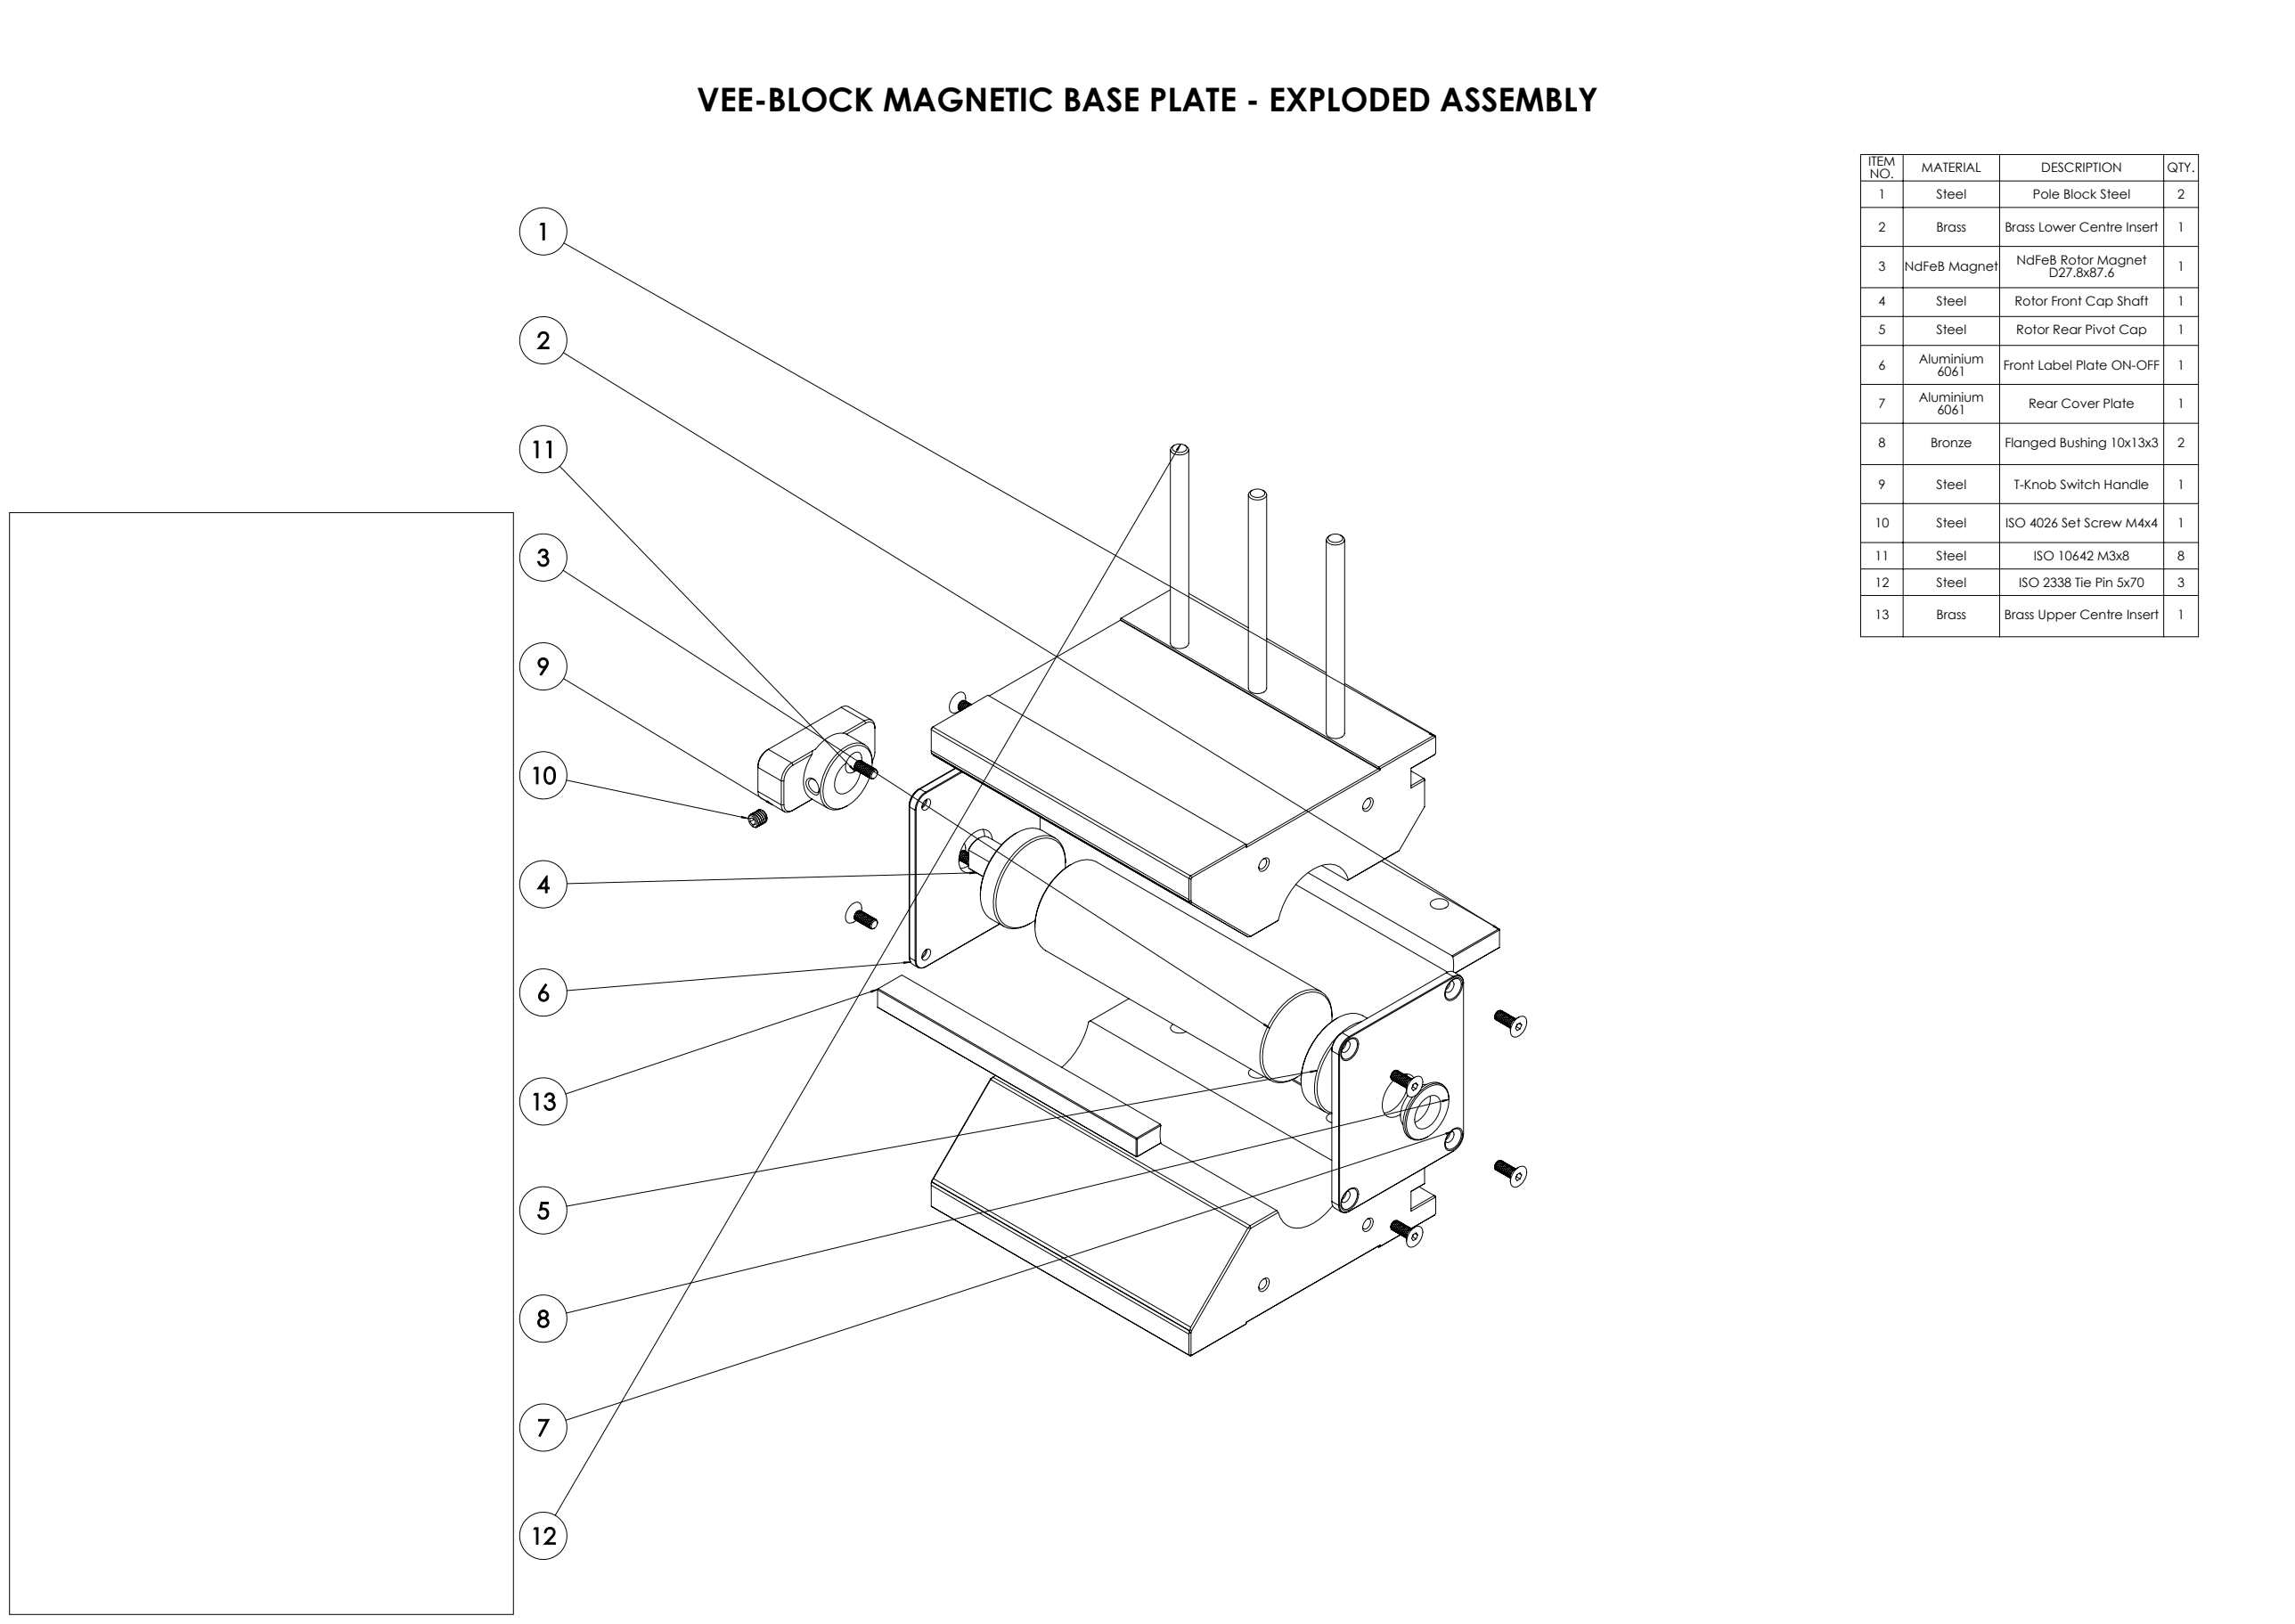
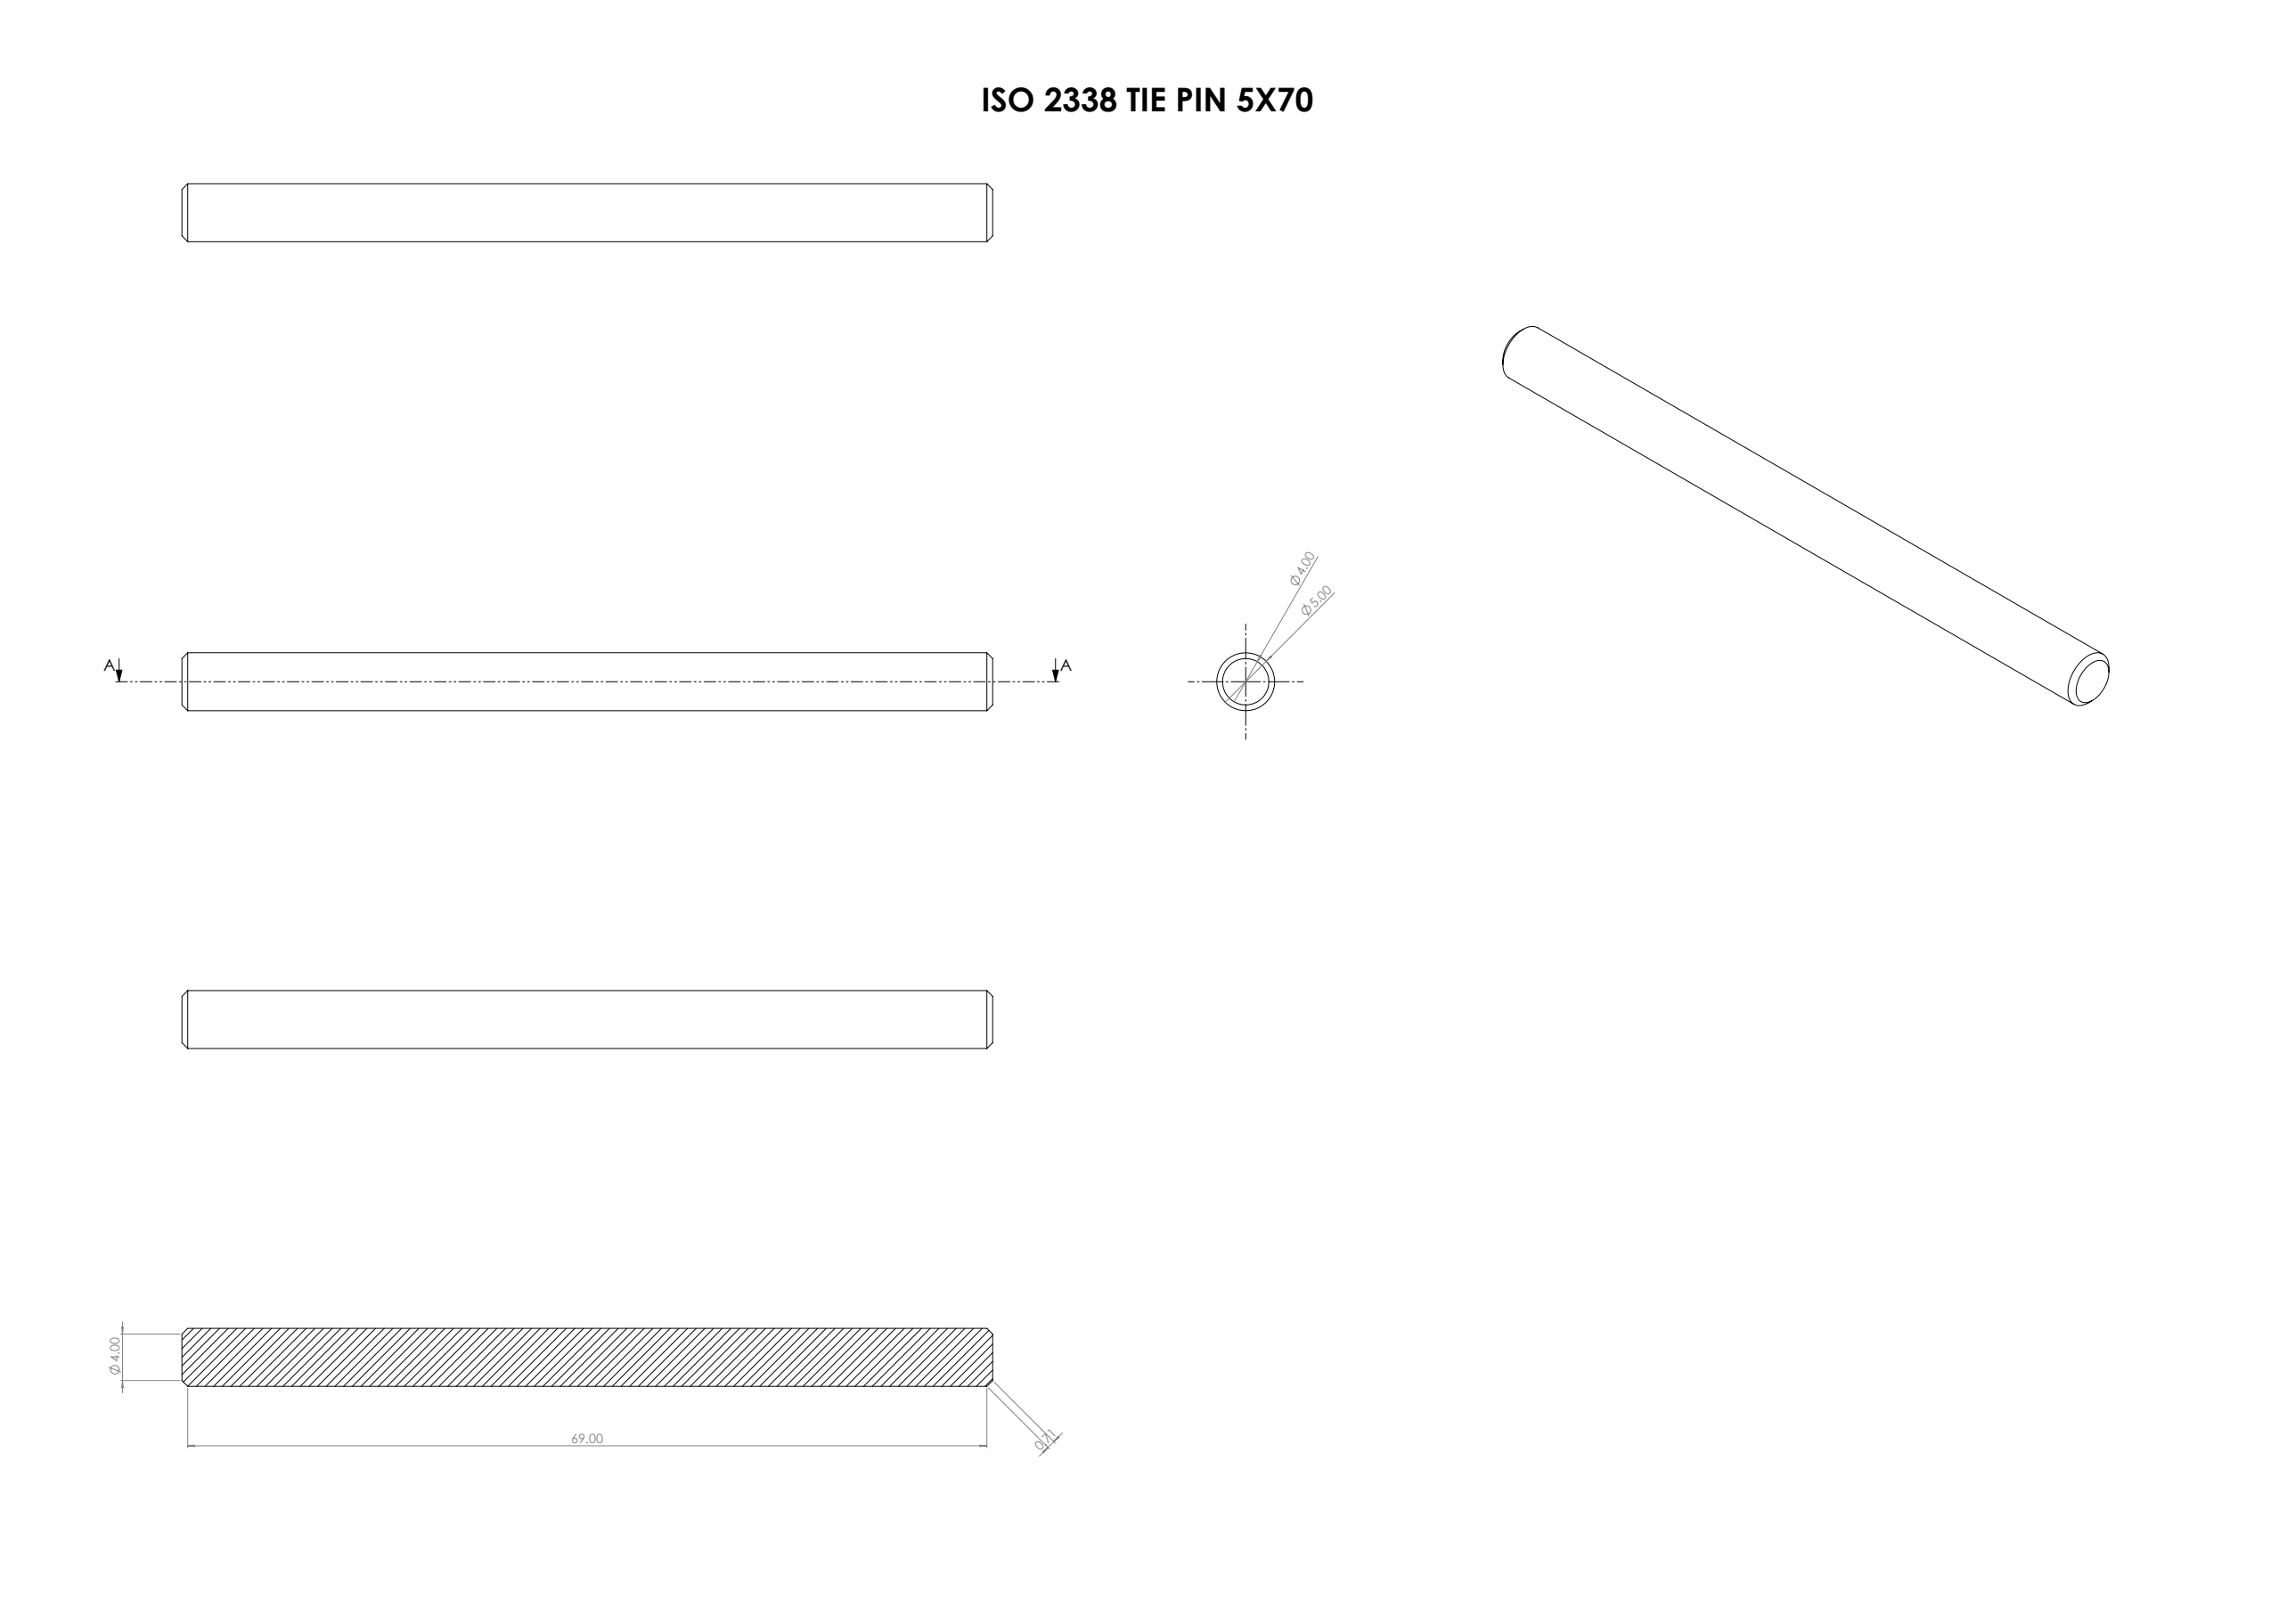
ISO-10303-21;
HEADER;
/* Generated by software containing ST-Developer
 * from STEP Tools, Inc. (www.steptools.com) 
 */

FILE_DESCRIPTION(
/* description */ (''),
/* implementation_level */ '2;1');

FILE_NAME(
/* name */ 'MAS-286',
/* time_stamp */ '2026-10-21T01:59:45-07:00',
/* author */ (''),
/* organization */ (''),
/* preprocessor_version */ 'ST-DEVELOPER v20.2',
/* originating_system */ 'Autodesk Translation Framework v15.15.0.0',
/* authorisation */ '');

FILE_SCHEMA (('AUTOMOTIVE_DESIGN { 1 0 10303 214 3 1 1 }'));
ENDSEC;

DATA;
#10=MECHANICAL_DESIGN_GEOMETRIC_PRESENTATION_REPRESENTATION('',(#463,#464,
#465,#466,#467,#468,#469,#470,#471,#472,#473,#474,#475,#476,#477,#478,#479,
#480),#18281);
#11=ITEM_DEFINED_TRANSFORMATION($,$,#9544,#9946);
#12=ITEM_DEFINED_TRANSFORMATION($,$,#9243,#9947);
#13=ITEM_DEFINED_TRANSFORMATION($,$,#9277,#9948);
#14=ITEM_DEFINED_TRANSFORMATION($,$,#9302,#9949);
#15=ITEM_DEFINED_TRANSFORMATION($,$,#9470,#9950);
#16=ITEM_DEFINED_TRANSFORMATION($,$,#9544,#9951);
#17=ITEM_DEFINED_TRANSFORMATION($,$,#9664,#9952);
#18=ITEM_DEFINED_TRANSFORMATION($,$,#9674,#9953);
#19=ITEM_DEFINED_TRANSFORMATION($,$,#9696,#9954);
#20=ITEM_DEFINED_TRANSFORMATION($,$,#9713,#9955);
#21=ITEM_DEFINED_TRANSFORMATION($,$,#9713,#9956);
#22=ITEM_DEFINED_TRANSFORMATION($,$,#9729,#9957);
#23=ITEM_DEFINED_TRANSFORMATION($,$,#9847,#9958);
#24=ITEM_DEFINED_TRANSFORMATION($,$,#9884,#9959);
#25=ITEM_DEFINED_TRANSFORMATION($,$,#9884,#9960);
#26=ITEM_DEFINED_TRANSFORMATION($,$,#9884,#9961);
#27=ITEM_DEFINED_TRANSFORMATION($,$,#9884,#9962);
#28=ITEM_DEFINED_TRANSFORMATION($,$,#9884,#9963);
#29=ITEM_DEFINED_TRANSFORMATION($,$,#9884,#9964);
#30=ITEM_DEFINED_TRANSFORMATION($,$,#9884,#9965);
#31=ITEM_DEFINED_TRANSFORMATION($,$,#9884,#9966);
#32=ITEM_DEFINED_TRANSFORMATION($,$,#9936,#9967);
#33=ITEM_DEFINED_TRANSFORMATION($,$,#9936,#9968);
#34=ITEM_DEFINED_TRANSFORMATION($,$,#9936,#9969);
#35=(
REPRESENTATION_RELATIONSHIP($,$,#18343,#18338)
REPRESENTATION_RELATIONSHIP_WITH_TRANSFORMATION(#11)
SHAPE_REPRESENTATION_RELATIONSHIP()
);
#36=(
REPRESENTATION_RELATIONSHIP($,$,#18339,#18338)
REPRESENTATION_RELATIONSHIP_WITH_TRANSFORMATION(#12)
SHAPE_REPRESENTATION_RELATIONSHIP()
);
#37=(
REPRESENTATION_RELATIONSHIP($,$,#18340,#18338)
REPRESENTATION_RELATIONSHIP_WITH_TRANSFORMATION(#13)
SHAPE_REPRESENTATION_RELATIONSHIP()
);
#38=(
REPRESENTATION_RELATIONSHIP($,$,#18341,#18338)
REPRESENTATION_RELATIONSHIP_WITH_TRANSFORMATION(#14)
SHAPE_REPRESENTATION_RELATIONSHIP()
);
#39=(
REPRESENTATION_RELATIONSHIP($,$,#18342,#18338)
REPRESENTATION_RELATIONSHIP_WITH_TRANSFORMATION(#15)
SHAPE_REPRESENTATION_RELATIONSHIP()
);
#40=(
REPRESENTATION_RELATIONSHIP($,$,#18343,#18338)
REPRESENTATION_RELATIONSHIP_WITH_TRANSFORMATION(#16)
SHAPE_REPRESENTATION_RELATIONSHIP()
);
#41=(
REPRESENTATION_RELATIONSHIP($,$,#18344,#18338)
REPRESENTATION_RELATIONSHIP_WITH_TRANSFORMATION(#17)
SHAPE_REPRESENTATION_RELATIONSHIP()
);
#42=(
REPRESENTATION_RELATIONSHIP($,$,#18345,#18338)
REPRESENTATION_RELATIONSHIP_WITH_TRANSFORMATION(#18)
SHAPE_REPRESENTATION_RELATIONSHIP()
);
#43=(
REPRESENTATION_RELATIONSHIP($,$,#18346,#18338)
REPRESENTATION_RELATIONSHIP_WITH_TRANSFORMATION(#19)
SHAPE_REPRESENTATION_RELATIONSHIP()
);
#44=(
REPRESENTATION_RELATIONSHIP($,$,#18347,#18338)
REPRESENTATION_RELATIONSHIP_WITH_TRANSFORMATION(#20)
SHAPE_REPRESENTATION_RELATIONSHIP()
);
#45=(
REPRESENTATION_RELATIONSHIP($,$,#18347,#18338)
REPRESENTATION_RELATIONSHIP_WITH_TRANSFORMATION(#21)
SHAPE_REPRESENTATION_RELATIONSHIP()
);
#46=(
REPRESENTATION_RELATIONSHIP($,$,#18348,#18338)
REPRESENTATION_RELATIONSHIP_WITH_TRANSFORMATION(#22)
SHAPE_REPRESENTATION_RELATIONSHIP()
);
#47=(
REPRESENTATION_RELATIONSHIP($,$,#18349,#18338)
REPRESENTATION_RELATIONSHIP_WITH_TRANSFORMATION(#23)
SHAPE_REPRESENTATION_RELATIONSHIP()
);
#48=(
REPRESENTATION_RELATIONSHIP($,$,#18350,#18338)
REPRESENTATION_RELATIONSHIP_WITH_TRANSFORMATION(#24)
SHAPE_REPRESENTATION_RELATIONSHIP()
);
#49=(
REPRESENTATION_RELATIONSHIP($,$,#18350,#18338)
REPRESENTATION_RELATIONSHIP_WITH_TRANSFORMATION(#25)
SHAPE_REPRESENTATION_RELATIONSHIP()
);
#50=(
REPRESENTATION_RELATIONSHIP($,$,#18350,#18338)
REPRESENTATION_RELATIONSHIP_WITH_TRANSFORMATION(#26)
SHAPE_REPRESENTATION_RELATIONSHIP()
);
#51=(
REPRESENTATION_RELATIONSHIP($,$,#18350,#18338)
REPRESENTATION_RELATIONSHIP_WITH_TRANSFORMATION(#27)
SHAPE_REPRESENTATION_RELATIONSHIP()
);
#52=(
REPRESENTATION_RELATIONSHIP($,$,#18350,#18338)
REPRESENTATION_RELATIONSHIP_WITH_TRANSFORMATION(#28)
SHAPE_REPRESENTATION_RELATIONSHIP()
);
#53=(
REPRESENTATION_RELATIONSHIP($,$,#18350,#18338)
REPRESENTATION_RELATIONSHIP_WITH_TRANSFORMATION(#29)
SHAPE_REPRESENTATION_RELATIONSHIP()
);
#54=(
REPRESENTATION_RELATIONSHIP($,$,#18350,#18338)
REPRESENTATION_RELATIONSHIP_WITH_TRANSFORMATION(#30)
SHAPE_REPRESENTATION_RELATIONSHIP()
);
#55=(
REPRESENTATION_RELATIONSHIP($,$,#18350,#18338)
REPRESENTATION_RELATIONSHIP_WITH_TRANSFORMATION(#31)
SHAPE_REPRESENTATION_RELATIONSHIP()
);
#56=(
REPRESENTATION_RELATIONSHIP($,$,#18351,#18338)
REPRESENTATION_RELATIONSHIP_WITH_TRANSFORMATION(#32)
SHAPE_REPRESENTATION_RELATIONSHIP()
);
#57=(
REPRESENTATION_RELATIONSHIP($,$,#18351,#18338)
REPRESENTATION_RELATIONSHIP_WITH_TRANSFORMATION(#33)
SHAPE_REPRESENTATION_RELATIONSHIP()
);
#58=(
REPRESENTATION_RELATIONSHIP($,$,#18351,#18338)
REPRESENTATION_RELATIONSHIP_WITH_TRANSFORMATION(#34)
SHAPE_REPRESENTATION_RELATIONSHIP()
);
#59=CONTEXT_DEPENDENT_SHAPE_REPRESENTATION(#35,#18314);
#60=CONTEXT_DEPENDENT_SHAPE_REPRESENTATION(#36,#18315);
#61=CONTEXT_DEPENDENT_SHAPE_REPRESENTATION(#37,#18316);
#62=CONTEXT_DEPENDENT_SHAPE_REPRESENTATION(#38,#18317);
#63=CONTEXT_DEPENDENT_SHAPE_REPRESENTATION(#39,#18318);
#64=CONTEXT_DEPENDENT_SHAPE_REPRESENTATION(#40,#18319);
#65=CONTEXT_DEPENDENT_SHAPE_REPRESENTATION(#41,#18320);
#66=CONTEXT_DEPENDENT_SHAPE_REPRESENTATION(#42,#18321);
#67=CONTEXT_DEPENDENT_SHAPE_REPRESENTATION(#43,#18322);
#68=CONTEXT_DEPENDENT_SHAPE_REPRESENTATION(#44,#18323);
#69=CONTEXT_DEPENDENT_SHAPE_REPRESENTATION(#45,#18324);
#70=CONTEXT_DEPENDENT_SHAPE_REPRESENTATION(#46,#18325);
#71=CONTEXT_DEPENDENT_SHAPE_REPRESENTATION(#47,#18326);
#72=CONTEXT_DEPENDENT_SHAPE_REPRESENTATION(#48,#18327);
#73=CONTEXT_DEPENDENT_SHAPE_REPRESENTATION(#49,#18328);
#74=CONTEXT_DEPENDENT_SHAPE_REPRESENTATION(#50,#18329);
#75=CONTEXT_DEPENDENT_SHAPE_REPRESENTATION(#51,#18330);
#76=CONTEXT_DEPENDENT_SHAPE_REPRESENTATION(#52,#18331);
#77=CONTEXT_DEPENDENT_SHAPE_REPRESENTATION(#53,#18332);
#78=CONTEXT_DEPENDENT_SHAPE_REPRESENTATION(#54,#18333);
#79=CONTEXT_DEPENDENT_SHAPE_REPRESENTATION(#55,#18334);
#80=CONTEXT_DEPENDENT_SHAPE_REPRESENTATION(#56,#18335);
#81=CONTEXT_DEPENDENT_SHAPE_REPRESENTATION(#57,#18336);
#82=CONTEXT_DEPENDENT_SHAPE_REPRESENTATION(#58,#18337);
#83=NEXT_ASSEMBLY_USAGE_OCCURRENCE('01_Pole_Block_Steel:1',
'01_Pole_Block_Steel:1','01_Pole_Block_Steel:1',#18353,#18358,
'01_Pole_Block_Steel:1');
#84=NEXT_ASSEMBLY_USAGE_OCCURRENCE('02_Brass_Lower_Centre_Insert:1',
'02_Brass_Lower_Centre_Insert:1','02_Brass_Lower_Centre_Insert:1',#18353,
#18354,'02_Brass_Lower_Centre_Insert:1');
#85=NEXT_ASSEMBLY_USAGE_OCCURRENCE('13_Brass_Upper_Centre_Insert:1',
'13_Brass_Upper_Centre_Insert:1','13_Brass_Upper_Centre_Insert:1',#18353,
#18355,'13_Brass_Upper_Centre_Insert:1');
#86=NEXT_ASSEMBLY_USAGE_OCCURRENCE('06_Front_Label_Plate_ON-OFF:1',
'06_Front_Label_Plate_ON-OFF:1','06_Front_Label_Plate_ON-OFF:1',#18353,
#18356,'06_Front_Label_Plate_ON-OFF:1');
#87=NEXT_ASSEMBLY_USAGE_OCCURRENCE('07_Rear_Cover_Plate:1',
'07_Rear_Cover_Plate:1','07_Rear_Cover_Plate:1',#18353,#18357,
'07_Rear_Cover_Plate:1');
#88=NEXT_ASSEMBLY_USAGE_OCCURRENCE('01_Pole_Block_Steel:2',
'01_Pole_Block_Steel:2','01_Pole_Block_Steel:2',#18353,#18358,
'01_Pole_Block_Steel:2');
#89=NEXT_ASSEMBLY_USAGE_OCCURRENCE('03_NdFeB_Rotor_Magnet_D27.8x87.6:2',
'03_NdFeB_Rotor_Magnet_D27.8x87.6:2',
'03_NdFeB_Rotor_Magnet_D27.8x87.6:2',#18353,#18359,
'03_NdFeB_Rotor_Magnet_D27.8x87.6:2');
#90=NEXT_ASSEMBLY_USAGE_OCCURRENCE('04_Rotor_Front_Cap_Shaft:2',
'04_Rotor_Front_Cap_Shaft:2','04_Rotor_Front_Cap_Shaft:2',#18353,#18360,
'04_Rotor_Front_Cap_Shaft:2');
#91=NEXT_ASSEMBLY_USAGE_OCCURRENCE('05_Rotor_Rear_Pivot_Cap:2',
'05_Rotor_Rear_Pivot_Cap:2','05_Rotor_Rear_Pivot_Cap:2',#18353,#18361,
'05_Rotor_Rear_Pivot_Cap:2');
#92=NEXT_ASSEMBLY_USAGE_OCCURRENCE('08_Flanged_Bushing_10x13x3:2',
'08_Flanged_Bushing_10x13x3:2','08_Flanged_Bushing_10x13x3:2',#18353,#18362,
'08_Flanged_Bushing_10x13x3:2');
#93=NEXT_ASSEMBLY_USAGE_OCCURRENCE('08_Flanged_Bushing_10x13x3:3',
'08_Flanged_Bushing_10x13x3:3','08_Flanged_Bushing_10x13x3:3',#18353,#18362,
'08_Flanged_Bushing_10x13x3:3');
#94=NEXT_ASSEMBLY_USAGE_OCCURRENCE('09_T-Knob_Switch_Handle:2',
'09_T-Knob_Switch_Handle:2','09_T-Knob_Switch_Handle:2',#18353,#18363,
'09_T-Knob_Switch_Handle:2');
#95=NEXT_ASSEMBLY_USAGE_OCCURRENCE('10_ISO_4026_Set_Screw_M4x4:2',
'10_ISO_4026_Set_Screw_M4x4:2','10_ISO_4026_Set_Screw_M4x4:2',#18353,#18364,
'10_ISO_4026_Set_Screw_M4x4:2');
#96=NEXT_ASSEMBLY_USAGE_OCCURRENCE('11_ISO_10642_M3x8:2',
'11_ISO_10642_M3x8:2','11_ISO_10642_M3x8:2',#18353,#18365,
'11_ISO_10642_M3x8:2');
#97=NEXT_ASSEMBLY_USAGE_OCCURRENCE('11_ISO_10642_M3x8:3',
'11_ISO_10642_M3x8:3','11_ISO_10642_M3x8:3',#18353,#18365,
'11_ISO_10642_M3x8:3');
#98=NEXT_ASSEMBLY_USAGE_OCCURRENCE('11_ISO_10642_M3x8:4',
'11_ISO_10642_M3x8:4','11_ISO_10642_M3x8:4',#18353,#18365,
'11_ISO_10642_M3x8:4');
#99=NEXT_ASSEMBLY_USAGE_OCCURRENCE('11_ISO_10642_M3x8:5',
'11_ISO_10642_M3x8:5','11_ISO_10642_M3x8:5',#18353,#18365,
'11_ISO_10642_M3x8:5');
#100=NEXT_ASSEMBLY_USAGE_OCCURRENCE('11_ISO_10642_M3x8:6',
'11_ISO_10642_M3x8:6','11_ISO_10642_M3x8:6',#18353,#18365,
'11_ISO_10642_M3x8:6');
#101=NEXT_ASSEMBLY_USAGE_OCCURRENCE('11_ISO_10642_M3x8:7',
'11_ISO_10642_M3x8:7','11_ISO_10642_M3x8:7',#18353,#18365,
'11_ISO_10642_M3x8:7');
#102=NEXT_ASSEMBLY_USAGE_OCCURRENCE('11_ISO_10642_M3x8:8',
'11_ISO_10642_M3x8:8','11_ISO_10642_M3x8:8',#18353,#18365,
'11_ISO_10642_M3x8:8');
#103=NEXT_ASSEMBLY_USAGE_OCCURRENCE('11_ISO_10642_M3x8:9',
'11_ISO_10642_M3x8:9','11_ISO_10642_M3x8:9',#18353,#18365,
'11_ISO_10642_M3x8:9');
#104=NEXT_ASSEMBLY_USAGE_OCCURRENCE('12_ISO_2338_Tie_Pin_5x70:2',
'12_ISO_2338_Tie_Pin_5x70:2','12_ISO_2338_Tie_Pin_5x70:2',#18353,#18366,
'12_ISO_2338_Tie_Pin_5x70:2');
#105=NEXT_ASSEMBLY_USAGE_OCCURRENCE('12_ISO_2338_Tie_Pin_5x70:3',
'12_ISO_2338_Tie_Pin_5x70:3','12_ISO_2338_Tie_Pin_5x70:3',#18353,#18366,
'12_ISO_2338_Tie_Pin_5x70:3');
#106=NEXT_ASSEMBLY_USAGE_OCCURRENCE('12_ISO_2338_Tie_Pin_5x70:4',
'12_ISO_2338_Tie_Pin_5x70:4','12_ISO_2338_Tie_Pin_5x70:4',#18353,#18366,
'12_ISO_2338_Tie_Pin_5x70:4');
#107=(
BOUNDED_CURVE()
B_SPLINE_CURVE(2,(#12695,#12696,#12697),.UNSPECIFIED.,.F.,.F.)
B_SPLINE_CURVE_WITH_KNOTS((3,3),(0.,0.110982483350979),.UNSPECIFIED.)
CURVE()
GEOMETRIC_REPRESENTATION_ITEM()
RATIONAL_B_SPLINE_CURVE((1.,1.,1.))
REPRESENTATION_ITEM('')
);
#108=(
BOUNDED_CURVE()
B_SPLINE_CURVE(2,(#12710,#12711,#12712),.UNSPECIFIED.,.F.,.F.)
B_SPLINE_CURVE_WITH_KNOTS((3,3),(0.058586025044114,0.117172050088227),
 .UNSPECIFIED.)
CURVE()
GEOMETRIC_REPRESENTATION_ITEM()
RATIONAL_B_SPLINE_CURVE((1.,1.,1.))
REPRESENTATION_ITEM('')
);
#109=(
BOUNDED_CURVE()
B_SPLINE_CURVE(2,(#12739,#12740,#12741),.UNSPECIFIED.,.F.,.F.)
B_SPLINE_CURVE_WITH_KNOTS((3,3),(0.,0.0585860250441136),.UNSPECIFIED.)
CURVE()
GEOMETRIC_REPRESENTATION_ITEM()
RATIONAL_B_SPLINE_CURVE((1.,1.,1.))
REPRESENTATION_ITEM('')
);
#110=(
BOUNDED_CURVE()
B_SPLINE_CURVE(2,(#12754,#12755,#12756),.UNSPECIFIED.,.F.,.F.)
B_SPLINE_CURVE_WITH_KNOTS((3,3),(0.0909175021833372,0.201899986183551),
 .UNSPECIFIED.)
CURVE()
GEOMETRIC_REPRESENTATION_ITEM()
RATIONAL_B_SPLINE_CURVE((1.,1.,1.))
REPRESENTATION_ITEM('')
);
#111=(
BOUNDED_CURVE()
B_SPLINE_CURVE(2,(#12765,#12766,#12767),.UNSPECIFIED.,.F.,.F.)
B_SPLINE_CURVE_WITH_KNOTS((3,3),(0.0485753412182672,0.117172050088219),
 .UNSPECIFIED.)
CURVE()
GEOMETRIC_REPRESENTATION_ITEM()
RATIONAL_B_SPLINE_CURVE((1.,1.,1.))
REPRESENTATION_ITEM('')
);
#112=(
BOUNDED_CURVE()
B_SPLINE_CURVE(2,(#12779,#12780,#12781),.UNSPECIFIED.,.F.,.F.)
B_SPLINE_CURVE_WITH_KNOTS((3,3),(0.0585860250445827,0.117172050088221),
 .UNSPECIFIED.)
CURVE()
GEOMETRIC_REPRESENTATION_ITEM()
RATIONAL_B_SPLINE_CURVE((1.,1.,1.))
REPRESENTATION_ITEM('')
);
#113=(
BOUNDED_CURVE()
B_SPLINE_CURVE(2,(#12785,#12786,#12787),.UNSPECIFIED.,.F.,.F.)
B_SPLINE_CURVE_WITH_KNOTS((3,3),(0.,0.068596708869952),.UNSPECIFIED.)
CURVE()
GEOMETRIC_REPRESENTATION_ITEM()
RATIONAL_B_SPLINE_CURVE((1.,1.,1.))
REPRESENTATION_ITEM('')
);
#114=(
BOUNDED_CURVE()
B_SPLINE_CURVE(2,(#12799,#12800,#12801),.UNSPECIFIED.,.F.,.F.)
B_SPLINE_CURVE_WITH_KNOTS((3,3),(0.0485753412182676,0.0585860250445827),
 .UNSPECIFIED.)
CURVE()
GEOMETRIC_REPRESENTATION_ITEM()
RATIONAL_B_SPLINE_CURVE((1.,1.,1.))
REPRESENTATION_ITEM('')
);
#115=(
BOUNDED_CURVE()
B_SPLINE_CURVE(2,(#13088,#13089,#13090),.UNSPECIFIED.,.F.,.F.)
B_SPLINE_CURVE_WITH_KNOTS((3,3),(0.058586025043638,0.0685967088699541),
 .UNSPECIFIED.)
CURVE()
GEOMETRIC_REPRESENTATION_ITEM()
RATIONAL_B_SPLINE_CURVE((1.,1.,1.))
REPRESENTATION_ITEM('')
);
#116=(
BOUNDED_CURVE()
B_SPLINE_CURVE(2,(#13101,#13102,#13103),.UNSPECIFIED.,.F.,.F.)
B_SPLINE_CURVE_WITH_KNOTS((3,3),(0.,0.058586025043638),.UNSPECIFIED.)
CURVE()
GEOMETRIC_REPRESENTATION_ITEM()
RATIONAL_B_SPLINE_CURVE((1.,1.,1.))
REPRESENTATION_ITEM('')
);
#117=(
BOUNDED_CURVE()
B_SPLINE_CURVE(2,(#14471,#14472,#14473),.UNSPECIFIED.,.F.,.F.)
B_SPLINE_CURVE_WITH_KNOTS((3,3),(0.,0.0727628528393549),.UNSPECIFIED.)
CURVE()
GEOMETRIC_REPRESENTATION_ITEM()
RATIONAL_B_SPLINE_CURVE((1.,1.,1.))
REPRESENTATION_ITEM('')
);
#118=(
BOUNDED_CURVE()
B_SPLINE_CURVE(2,(#14477,#14478,#14479),.UNSPECIFIED.,.F.,.F.)
B_SPLINE_CURVE_WITH_KNOTS((3,3),(0.,0.0727628528393549),.UNSPECIFIED.)
CURVE()
GEOMETRIC_REPRESENTATION_ITEM()
RATIONAL_B_SPLINE_CURVE((1.,1.,1.))
REPRESENTATION_ITEM('')
);
#119=(
BOUNDED_CURVE()
B_SPLINE_CURVE(2,(#14814,#14815,#14816),.UNSPECIFIED.,.F.,.F.)
B_SPLINE_CURVE_WITH_KNOTS((3,3),(0.,0.0729284032695322),.UNSPECIFIED.)
CURVE()
GEOMETRIC_REPRESENTATION_ITEM()
RATIONAL_B_SPLINE_CURVE((1.,1.,1.))
REPRESENTATION_ITEM('')
);
#120=(
BOUNDED_CURVE()
B_SPLINE_CURVE(2,(#14820,#14821,#14822),.UNSPECIFIED.,.F.,.F.)
B_SPLINE_CURVE_WITH_KNOTS((3,3),(0.,0.072928403269532),.UNSPECIFIED.)
CURVE()
GEOMETRIC_REPRESENTATION_ITEM()
RATIONAL_B_SPLINE_CURVE((1.,1.,1.))
REPRESENTATION_ITEM('')
);
#121=(
BOUNDED_CURVE()
B_SPLINE_CURVE(2,(#14826,#14827,#14828),.UNSPECIFIED.,.F.,.F.)
B_SPLINE_CURVE_WITH_KNOTS((3,3),(0.,0.0457691166614135),.UNSPECIFIED.)
CURVE()
GEOMETRIC_REPRESENTATION_ITEM()
RATIONAL_B_SPLINE_CURVE((1.,1.,1.))
REPRESENTATION_ITEM('')
);
#122=(
BOUNDED_CURVE()
B_SPLINE_CURVE(2,(#14831,#14832,#14833),.UNSPECIFIED.,.F.,.F.)
B_SPLINE_CURVE_WITH_KNOTS((3,3),(0.,0.0457691166614134),.UNSPECIFIED.)
CURVE()
GEOMETRIC_REPRESENTATION_ITEM()
RATIONAL_B_SPLINE_CURVE((1.,1.,1.))
REPRESENTATION_ITEM('')
);
#123=(
BOUNDED_CURVE()
B_SPLINE_CURVE(2,(#14897,#14898,#14899),.UNSPECIFIED.,.F.,.F.)
B_SPLINE_CURVE_WITH_KNOTS((3,3),(0.,0.0577818255968905),.UNSPECIFIED.)
CURVE()
GEOMETRIC_REPRESENTATION_ITEM()
RATIONAL_B_SPLINE_CURVE((1.,1.,1.))
REPRESENTATION_ITEM('')
);
#124=(
BOUNDED_CURVE()
B_SPLINE_CURVE(2,(#14903,#14904,#14905),.UNSPECIFIED.,.F.,.F.)
B_SPLINE_CURVE_WITH_KNOTS((3,3),(0.,0.0577818255968905),.UNSPECIFIED.)
CURVE()
GEOMETRIC_REPRESENTATION_ITEM()
RATIONAL_B_SPLINE_CURVE((1.,1.,1.))
REPRESENTATION_ITEM('')
);
#125=(
BOUNDED_CURVE()
B_SPLINE_CURVE(2,(#14909,#14910,#14911),.UNSPECIFIED.,.F.,.F.)
B_SPLINE_CURVE_WITH_KNOTS((3,3),(0.,0.0492830096737056),.UNSPECIFIED.)
CURVE()
GEOMETRIC_REPRESENTATION_ITEM()
RATIONAL_B_SPLINE_CURVE((1.,1.,1.))
REPRESENTATION_ITEM('')
);
#126=(
BOUNDED_CURVE()
B_SPLINE_CURVE(2,(#14914,#14915,#14916),.UNSPECIFIED.,.F.,.F.)
B_SPLINE_CURVE_WITH_KNOTS((3,3),(0.,0.0492830096737056),.UNSPECIFIED.)
CURVE()
GEOMETRIC_REPRESENTATION_ITEM()
RATIONAL_B_SPLINE_CURVE((1.,1.,1.))
REPRESENTATION_ITEM('')
);
#127=(
BOUNDED_CURVE()
B_SPLINE_CURVE(2,(#14920,#14921,#14922),.UNSPECIFIED.,.F.,.F.)
B_SPLINE_CURVE_WITH_KNOTS((3,3),(0.,0.072928403269532),.UNSPECIFIED.)
CURVE()
GEOMETRIC_REPRESENTATION_ITEM()
RATIONAL_B_SPLINE_CURVE((1.,1.,1.))
REPRESENTATION_ITEM('')
);
#128=(
BOUNDED_CURVE()
B_SPLINE_CURVE(2,(#14926,#14927,#14928),.UNSPECIFIED.,.F.,.F.)
B_SPLINE_CURVE_WITH_KNOTS((3,3),(0.,0.0729284032695322),.UNSPECIFIED.)
CURVE()
GEOMETRIC_REPRESENTATION_ITEM()
RATIONAL_B_SPLINE_CURVE((1.,1.,1.))
REPRESENTATION_ITEM('')
);
#129=(
BOUNDED_CURVE()
B_SPLINE_CURVE(2,(#14932,#14933,#14934),.UNSPECIFIED.,.F.,.F.)
B_SPLINE_CURVE_WITH_KNOTS((3,3),(0.,0.0457691166614135),.UNSPECIFIED.)
CURVE()
GEOMETRIC_REPRESENTATION_ITEM()
RATIONAL_B_SPLINE_CURVE((1.,1.,1.))
REPRESENTATION_ITEM('')
);
#130=(
BOUNDED_CURVE()
B_SPLINE_CURVE(2,(#14937,#14938,#14939),.UNSPECIFIED.,.F.,.F.)
B_SPLINE_CURVE_WITH_KNOTS((3,3),(0.,0.0457691166614134),.UNSPECIFIED.)
CURVE()
GEOMETRIC_REPRESENTATION_ITEM()
RATIONAL_B_SPLINE_CURVE((1.,1.,1.))
REPRESENTATION_ITEM('')
);
#131=(
BOUNDED_CURVE()
B_SPLINE_CURVE(2,(#14973,#14974,#14975),.UNSPECIFIED.,.F.,.F.)
B_SPLINE_CURVE_WITH_KNOTS((3,3),(0.,0.210313307559557),.UNSPECIFIED.)
CURVE()
GEOMETRIC_REPRESENTATION_ITEM()
RATIONAL_B_SPLINE_CURVE((1.,1.,1.))
REPRESENTATION_ITEM('')
);
#132=(
BOUNDED_CURVE()
B_SPLINE_CURVE(2,(#14979,#14980,#14981),.UNSPECIFIED.,.F.,.F.)
B_SPLINE_CURVE_WITH_KNOTS((3,3),(0.210313307559557,0.420626615119114),
 .UNSPECIFIED.)
CURVE()
GEOMETRIC_REPRESENTATION_ITEM()
RATIONAL_B_SPLINE_CURVE((1.,1.,1.))
REPRESENTATION_ITEM('')
);
#133=(
BOUNDED_CURVE()
B_SPLINE_CURVE(2,(#14985,#14986,#14987),.UNSPECIFIED.,.F.,.F.)
B_SPLINE_CURVE_WITH_KNOTS((3,3),(0.,0.0433664286594662),.UNSPECIFIED.)
CURVE()
GEOMETRIC_REPRESENTATION_ITEM()
RATIONAL_B_SPLINE_CURVE((1.,1.,1.))
REPRESENTATION_ITEM('')
);
#134=(
BOUNDED_CURVE()
B_SPLINE_CURVE(2,(#14990,#14991,#14992),.UNSPECIFIED.,.F.,.F.)
B_SPLINE_CURVE_WITH_KNOTS((3,3),(0.,0.0433664286594663),.UNSPECIFIED.)
CURVE()
GEOMETRIC_REPRESENTATION_ITEM()
RATIONAL_B_SPLINE_CURVE((1.,1.,1.))
REPRESENTATION_ITEM('')
);
#135=(
BOUNDED_CURVE()
B_SPLINE_CURVE(2,(#15011,#15012,#15013),.UNSPECIFIED.,.F.,.F.)
B_SPLINE_CURVE_WITH_KNOTS((3,3),(0.,0.0577818255968905),.UNSPECIFIED.)
CURVE()
GEOMETRIC_REPRESENTATION_ITEM()
RATIONAL_B_SPLINE_CURVE((1.,1.,1.))
REPRESENTATION_ITEM('')
);
#136=(
BOUNDED_CURVE()
B_SPLINE_CURVE(2,(#15017,#15018,#15019),.UNSPECIFIED.,.F.,.F.)
B_SPLINE_CURVE_WITH_KNOTS((3,3),(0.,0.0577818255968905),.UNSPECIFIED.)
CURVE()
GEOMETRIC_REPRESENTATION_ITEM()
RATIONAL_B_SPLINE_CURVE((1.,1.,1.))
REPRESENTATION_ITEM('')
);
#137=(
BOUNDED_CURVE()
B_SPLINE_CURVE(2,(#15023,#15024,#15025),.UNSPECIFIED.,.F.,.F.)
B_SPLINE_CURVE_WITH_KNOTS((3,3),(0.,0.0492830096737056),.UNSPECIFIED.)
CURVE()
GEOMETRIC_REPRESENTATION_ITEM()
RATIONAL_B_SPLINE_CURVE((1.,1.,1.))
REPRESENTATION_ITEM('')
);
#138=(
BOUNDED_CURVE()
B_SPLINE_CURVE(2,(#15028,#15029,#15030),.UNSPECIFIED.,.F.,.F.)
B_SPLINE_CURVE_WITH_KNOTS((3,3),(0.,0.0492830096737056),.UNSPECIFIED.)
CURVE()
GEOMETRIC_REPRESENTATION_ITEM()
RATIONAL_B_SPLINE_CURVE((1.,1.,1.))
REPRESENTATION_ITEM('')
);
#139=(
BOUNDED_CURVE()
B_SPLINE_CURVE(2,(#15034,#15035,#15036),.UNSPECIFIED.,.F.,.F.)
B_SPLINE_CURVE_WITH_KNOTS((3,3),(0.,0.0433664286594662),.UNSPECIFIED.)
CURVE()
GEOMETRIC_REPRESENTATION_ITEM()
RATIONAL_B_SPLINE_CURVE((1.,1.,1.))
REPRESENTATION_ITEM('')
);
#140=(
BOUNDED_CURVE()
B_SPLINE_CURVE(2,(#15040,#15041,#15042),.UNSPECIFIED.,.F.,.F.)
B_SPLINE_CURVE_WITH_KNOTS((3,3),(0.,0.0433664286594662),.UNSPECIFIED.)
CURVE()
GEOMETRIC_REPRESENTATION_ITEM()
RATIONAL_B_SPLINE_CURVE((1.,1.,1.))
REPRESENTATION_ITEM('')
);
#141=(
BOUNDED_CURVE()
B_SPLINE_CURVE(2,(#15046,#15047,#15048),.UNSPECIFIED.,.F.,.F.)
B_SPLINE_CURVE_WITH_KNOTS((3,3),(0.210313307559558,0.420626615119116),
 .UNSPECIFIED.)
CURVE()
GEOMETRIC_REPRESENTATION_ITEM()
RATIONAL_B_SPLINE_CURVE((1.,1.,1.))
REPRESENTATION_ITEM('')
);
#142=(
BOUNDED_CURVE()
B_SPLINE_CURVE(2,(#15051,#15052,#15053),.UNSPECIFIED.,.F.,.F.)
B_SPLINE_CURVE_WITH_KNOTS((3,3),(0.,0.210313307559558),.UNSPECIFIED.)
CURVE()
GEOMETRIC_REPRESENTATION_ITEM()
RATIONAL_B_SPLINE_CURVE((1.,1.,1.))
REPRESENTATION_ITEM('')
);
#143=B_SPLINE_SURFACE_WITH_KNOTS('',2,1,((#12638,#12639),(#12640,#12641),
(#12642,#12643),(#12644,#12645),(#12646,#12647),(#12648,#12649),(#12650,
#12651)),.UNSPECIFIED.,.F.,.F.,.F.,(3,2,2,3),(2,2),(-1.09408743911249,0.,
1.,1.84668421503224),(-0.0908822509939087,0.140882250993909),
 .UNSPECIFIED.);
#144=B_SPLINE_SURFACE_WITH_KNOTS('',2,1,((#13225,#13226),(#13227,#13228),
(#13229,#13230),(#13231,#13232),(#13233,#13234),(#13235,#13236),(#13237,
#13238)),.UNSPECIFIED.,.F.,.F.,.F.,(3,2,2,3),(2,2),(-0.763868143299771,
0.,1.,1.96021762995607),(-0.090882250993909,0.140882250993909),
 .UNSPECIFIED.);
#145=B_SPLINE_SURFACE_WITH_KNOTS('',2,1,((#13240,#13241),(#13242,#13243),
(#13244,#13245)),.UNSPECIFIED.,.F.,.F.,.F.,(3,3),(2,2),(0.,1.),(0.,0.025),
 .UNSPECIFIED.);
#146=B_SPLINE_SURFACE_WITH_KNOTS('',2,1,((#13247,#13248),(#13249,#13250),
(#13251,#13252)),.UNSPECIFIED.,.F.,.F.,.F.,(3,3),(2,2),(0.,1.),(0.,0.025),
 .UNSPECIFIED.);
#147=B_SPLINE_SURFACE_WITH_KNOTS('',2,1,((#13254,#13255),(#13256,#13257),
(#13258,#13259)),.UNSPECIFIED.,.F.,.F.,.F.,(3,3),(2,2),(0.,1.),(0.,0.025),
 .UNSPECIFIED.);
#148=B_SPLINE_SURFACE_WITH_KNOTS('',2,1,((#13261,#13262),(#13263,#13264),
(#13265,#13266)),.UNSPECIFIED.,.F.,.F.,.F.,(3,3),(2,2),(0.,1.),(0.,0.025),
 .UNSPECIFIED.);
#149=B_SPLINE_SURFACE_WITH_KNOTS('',2,1,((#13268,#13269),(#13270,#13271),
(#13272,#13273)),.UNSPECIFIED.,.F.,.F.,.F.,(3,3),(2,2),(0.,1.),(0.,0.025),
 .UNSPECIFIED.);
#150=B_SPLINE_SURFACE_WITH_KNOTS('',2,1,((#13356,#13357),(#13358,#13359),
(#13360,#13361)),.UNSPECIFIED.,.F.,.F.,.F.,(3,3),(2,2),(0.,1.),(0.,0.025),
 .UNSPECIFIED.);
#151=B_SPLINE_SURFACE_WITH_KNOTS('',2,1,((#13369,#13370),(#13371,#13372),
(#13373,#13374)),.UNSPECIFIED.,.F.,.F.,.F.,(3,3),(2,2),(0.,1.),(0.,0.025),
 .UNSPECIFIED.);
#152=B_SPLINE_SURFACE_WITH_KNOTS('',2,1,((#13380,#13381),(#13382,#13383),
(#13384,#13385)),.UNSPECIFIED.,.F.,.F.,.F.,(3,3),(2,2),(0.,1.),(0.,0.025),
 .UNSPECIFIED.);
#153=B_SPLINE_SURFACE_WITH_KNOTS('',2,1,((#13391,#13392),(#13393,#13394),
(#13395,#13396)),.UNSPECIFIED.,.F.,.F.,.F.,(3,3),(2,2),(0.,1.),(0.,0.025),
 .UNSPECIFIED.);
#154=B_SPLINE_SURFACE_WITH_KNOTS('',2,1,((#13402,#13403),(#13404,#13405),
(#13406,#13407)),.UNSPECIFIED.,.F.,.F.,.F.,(3,3),(2,2),(0.,1.),(0.,0.025),
 .UNSPECIFIED.);
#155=B_SPLINE_SURFACE_WITH_KNOTS('',2,1,((#13413,#13414),(#13415,#13416),
(#13417,#13418)),.UNSPECIFIED.,.F.,.F.,.F.,(3,3),(2,2),(0.,1.),(0.,0.025),
 .UNSPECIFIED.);
#156=B_SPLINE_SURFACE_WITH_KNOTS('',2,1,((#13424,#13425),(#13426,#13427),
(#13428,#13429)),.UNSPECIFIED.,.F.,.F.,.F.,(3,3),(2,2),(0.,1.),(0.,0.025),
 .UNSPECIFIED.);
#157=B_SPLINE_SURFACE_WITH_KNOTS('',2,1,((#13435,#13436),(#13437,#13438),
(#13439,#13440)),.UNSPECIFIED.,.F.,.F.,.F.,(3,3),(2,2),(0.,1.),(0.,0.025),
 .UNSPECIFIED.);
#158=B_SPLINE_SURFACE_WITH_KNOTS('',2,1,((#13446,#13447),(#13448,#13449),
(#13450,#13451)),.UNSPECIFIED.,.F.,.F.,.F.,(3,3),(2,2),(0.,1.),(0.,0.025),
 .UNSPECIFIED.);
#159=B_SPLINE_SURFACE_WITH_KNOTS('',2,1,((#13457,#13458),(#13459,#13460),
(#13461,#13462)),.UNSPECIFIED.,.F.,.F.,.F.,(3,3),(2,2),(0.,1.),(0.,0.025),
 .UNSPECIFIED.);
#160=B_SPLINE_SURFACE_WITH_KNOTS('',2,1,((#13468,#13469),(#13470,#13471),
(#13472,#13473)),.UNSPECIFIED.,.F.,.F.,.F.,(3,3),(2,2),(0.,1.),(0.,0.025),
 .UNSPECIFIED.);
#161=B_SPLINE_SURFACE_WITH_KNOTS('',2,1,((#13519,#13520),(#13521,#13522),
(#13523,#13524)),.UNSPECIFIED.,.F.,.F.,.F.,(3,3),(2,2),(0.,1.),(0.,0.025),
 .UNSPECIFIED.);
#162=B_SPLINE_SURFACE_WITH_KNOTS('',2,1,((#13532,#13533),(#13534,#13535),
(#13536,#13537)),.UNSPECIFIED.,.F.,.F.,.F.,(3,3),(2,2),(0.,1.),(0.,0.025),
 .UNSPECIFIED.);
#163=B_SPLINE_SURFACE_WITH_KNOTS('',2,1,((#13543,#13544),(#13545,#13546),
(#13547,#13548)),.UNSPECIFIED.,.F.,.F.,.F.,(3,3),(2,2),(0.,1.),(0.,0.025),
 .UNSPECIFIED.);
#164=B_SPLINE_SURFACE_WITH_KNOTS('',2,1,((#13554,#13555),(#13556,#13557),
(#13558,#13559)),.UNSPECIFIED.,.F.,.F.,.F.,(3,3),(2,2),(0.,1.),(0.,0.025),
 .UNSPECIFIED.);
#165=B_SPLINE_SURFACE_WITH_KNOTS('',2,1,((#13565,#13566),(#13567,#13568),
(#13569,#13570)),.UNSPECIFIED.,.F.,.F.,.F.,(3,3),(2,2),(0.,1.),(0.,0.025),
 .UNSPECIFIED.);
#166=B_SPLINE_SURFACE_WITH_KNOTS('',2,1,((#13576,#13577),(#13578,#13579),
(#13580,#13581)),.UNSPECIFIED.,.F.,.F.,.F.,(3,3),(2,2),(0.,1.),(0.,0.025),
 .UNSPECIFIED.);
#167=B_SPLINE_SURFACE_WITH_KNOTS('',2,1,((#13587,#13588),(#13589,#13590),
(#13591,#13592)),.UNSPECIFIED.,.F.,.F.,.F.,(3,3),(2,2),(0.,1.),(0.,0.025),
 .UNSPECIFIED.);
#168=B_SPLINE_SURFACE_WITH_KNOTS('',2,1,((#13598,#13599),(#13600,#13601),
(#13602,#13603)),.UNSPECIFIED.,.F.,.F.,.F.,(3,3),(2,2),(0.,1.),(0.,0.025),
 .UNSPECIFIED.);
#169=B_SPLINE_SURFACE_WITH_KNOTS('',2,1,((#13609,#13610),(#13611,#13612),
(#13613,#13614)),.UNSPECIFIED.,.F.,.F.,.F.,(3,3),(2,2),(0.,1.),(0.,0.025),
 .UNSPECIFIED.);
#170=B_SPLINE_SURFACE_WITH_KNOTS('',2,1,((#13620,#13621),(#13622,#13623),
(#13624,#13625)),.UNSPECIFIED.,.F.,.F.,.F.,(3,3),(2,2),(0.,1.),(0.,0.025),
 .UNSPECIFIED.);
#171=B_SPLINE_SURFACE_WITH_KNOTS('',2,1,((#13631,#13632),(#13633,#13634),
(#13635,#13636)),.UNSPECIFIED.,.F.,.F.,.F.,(3,3),(2,2),(0.,1.),(0.,0.025),
 .UNSPECIFIED.);
#172=B_SPLINE_SURFACE_WITH_KNOTS('',2,1,((#13682,#13683),(#13684,#13685),
(#13686,#13687)),.UNSPECIFIED.,.F.,.F.,.F.,(3,3),(2,2),(0.,1.),(0.,0.025),
 .UNSPECIFIED.);
#173=B_SPLINE_SURFACE_WITH_KNOTS('',2,1,((#13695,#13696),(#13697,#13698),
(#13699,#13700)),.UNSPECIFIED.,.F.,.F.,.F.,(3,3),(2,2),(0.,1.),(0.,0.025),
 .UNSPECIFIED.);
#174=B_SPLINE_SURFACE_WITH_KNOTS('',2,1,((#13706,#13707),(#13708,#13709),
(#13710,#13711)),.UNSPECIFIED.,.F.,.F.,.F.,(3,3),(2,2),(0.,1.),(0.,0.025),
 .UNSPECIFIED.);
#175=B_SPLINE_SURFACE_WITH_KNOTS('',2,1,((#13717,#13718),(#13719,#13720),
(#13721,#13722)),.UNSPECIFIED.,.F.,.F.,.F.,(3,3),(2,2),(0.,1.),(0.,0.025),
 .UNSPECIFIED.);
#176=B_SPLINE_SURFACE_WITH_KNOTS('',2,1,((#13728,#13729),(#13730,#13731),
(#13732,#13733)),.UNSPECIFIED.,.F.,.F.,.F.,(3,3),(2,2),(0.,1.),(0.,0.025),
 .UNSPECIFIED.);
#177=B_SPLINE_SURFACE_WITH_KNOTS('',2,1,((#13739,#13740),(#13741,#13742),
(#13743,#13744)),.UNSPECIFIED.,.F.,.F.,.F.,(3,3),(2,2),(0.,1.),(0.,0.025),
 .UNSPECIFIED.);
#178=B_SPLINE_SURFACE_WITH_KNOTS('',2,1,((#13750,#13751),(#13752,#13753),
(#13754,#13755)),.UNSPECIFIED.,.F.,.F.,.F.,(3,3),(2,2),(0.,1.),(0.,0.025),
 .UNSPECIFIED.);
#179=B_SPLINE_SURFACE_WITH_KNOTS('',2,1,((#13761,#13762),(#13763,#13764),
(#13765,#13766)),.UNSPECIFIED.,.F.,.F.,.F.,(3,3),(2,2),(0.,1.),(0.,0.025),
 .UNSPECIFIED.);
#180=B_SPLINE_SURFACE_WITH_KNOTS('',2,1,((#13772,#13773),(#13774,#13775),
(#13776,#13777)),.UNSPECIFIED.,.F.,.F.,.F.,(3,3),(2,2),(0.,1.),(0.,0.025),
 .UNSPECIFIED.);
#181=B_SPLINE_SURFACE_WITH_KNOTS('',2,1,((#13783,#13784),(#13785,#13786),
(#13787,#13788)),.UNSPECIFIED.,.F.,.F.,.F.,(3,3),(2,2),(0.,1.),(0.,0.025),
 .UNSPECIFIED.);
#182=B_SPLINE_SURFACE_WITH_KNOTS('',2,1,((#13794,#13795),(#13796,#13797),
(#13798,#13799)),.UNSPECIFIED.,.F.,.F.,.F.,(3,3),(2,2),(0.,1.),(0.,0.025),
 .UNSPECIFIED.);
#183=B_SPLINE_SURFACE_WITH_KNOTS('',3,3,((#14625,#14626,#14627,#14628,#14629,
#14630,#14631,#14632,#14633,#14634,#14635,#14636,#14637,#14638,#14639,#14640,
#14641,#14642,#14643,#14644),(#14645,#14646,#14647,#14648,#14649,#14650,
#14651,#14652,#14653,#14654,#14655,#14656,#14657,#14658,#14659,#14660,#14661,
#14662,#14663,#14664),(#14665,#14666,#14667,#14668,#14669,#14670,#14671,
#14672,#14673,#14674,#14675,#14676,#14677,#14678,#14679,#14680,#14681,#14682,
#14683,#14684),(#14685,#14686,#14687,#14688,#14689,#14690,#14691,#14692,
#14693,#14694,#14695,#14696,#14697,#14698,#14699,#14700,#14701,#14702,#14703,
#14704)),.UNSPECIFIED.,.F.,.T.,.F.,(4,4),(4,1,1,1,1,1,1,1,1,1,1,1,1,1,1,
1,1,4),(0.,1.),(0.929489890414013,1.01801273712011,1.06227416047316,1.10653558382621,
1.1950584305323,1.2835812772384,1.3721041239445,1.41636554729754,1.46062697065059,
1.54914981735669,1.63767266406279,1.68193408741583,1.72619551076888,1.81471835747498,
1.90324120418107,1.99176405088717,2.08028689759327,2.16880974429936),
 .UNSPECIFIED.);
#184=B_SPLINE_SURFACE_WITH_KNOTS('',3,3,((#15681,#15682,#15683,#15684,#15685,
#15686,#15687,#15688,#15689,#15690,#15691,#15692,#15693,#15694,#15695,#15696,
#15697,#15698,#15699,#15700,#15701,#15702,#15703,#15704,#15705,#15706,#15707,
#15708,#15709,#15710,#15711,#15712,#15713,#15714,#15715),(#15716,#15717,
#15718,#15719,#15720,#15721,#15722,#15723,#15724,#15725,#15726,#15727,#15728,
#15729,#15730,#15731,#15732,#15733,#15734,#15735,#15736,#15737,#15738,#15739,
#15740,#15741,#15742,#15743,#15744,#15745,#15746,#15747,#15748,#15749,#15750),
(#15751,#15752,#15753,#15754,#15755,#15756,#15757,#15758,#15759,#15760,
#15761,#15762,#15763,#15764,#15765,#15766,#15767,#15768,#15769,#15770,#15771,
#15772,#15773,#15774,#15775,#15776,#15777,#15778,#15779,#15780,#15781,#15782,
#15783,#15784,#15785),(#15786,#15787,#15788,#15789,#15790,#15791,#15792,
#15793,#15794,#15795,#15796,#15797,#15798,#15799,#15800,#15801,#15802,#15803,
#15804,#15805,#15806,#15807,#15808,#15809,#15810,#15811,#15812,#15813,#15814,
#15815,#15816,#15817,#15818,#15819,#15820)),.UNSPECIFIED.,.F.,.F.,.F.,(4,
4),(4,1,1,1,1,1,1,1,1,1,1,1,1,1,1,1,1,1,1,1,1,1,1,1,1,1,1,1,1,1,1,1,4),
(0.,0.0460148164544132),(8.31058692273978,9.29852639258487,10.28646586243,
11.274405332275,12.2623448021201,13.2502842719652,14.2382237418103,15.2261632116554,
16.2141026815005,17.2020421513455,18.1899816211906,19.1779210910357,20.1658605608808,
21.1538000307259,22.141739500571,23.129678970416,24.1176184402611,25.1055579101062,
26.0934973799513,27.0814368497964,28.0693763196415,29.0573157894865,30.0452552593316,
31.0331947291767,32.0211341990218,33.0090736688669,33.997013138712,34.9849526085571,
35.9728920784021,36.9608315482472,37.9487710180923,38.9367104879374,39.9246499577825),
 .UNSPECIFIED.);
#185=B_SPLINE_SURFACE_WITH_KNOTS('',3,3,((#16035,#16036,#16037,#16038,#16039,
#16040,#16041,#16042,#16043,#16044,#16045,#16046,#16047,#16048,#16049,#16050,
#16051,#16052,#16053,#16054,#16055,#16056,#16057,#16058,#16059,#16060,#16061,
#16062,#16063,#16064,#16065,#16066,#16067,#16068,#16069),(#16070,#16071,
#16072,#16073,#16074,#16075,#16076,#16077,#16078,#16079,#16080,#16081,#16082,
#16083,#16084,#16085,#16086,#16087,#16088,#16089,#16090,#16091,#16092,#16093,
#16094,#16095,#16096,#16097,#16098,#16099,#16100,#16101,#16102,#16103,#16104),
(#16105,#16106,#16107,#16108,#16109,#16110,#16111,#16112,#16113,#16114,
#16115,#16116,#16117,#16118,#16119,#16120,#16121,#16122,#16123,#16124,#16125,
#16126,#16127,#16128,#16129,#16130,#16131,#16132,#16133,#16134,#16135,#16136,
#16137,#16138,#16139),(#16140,#16141,#16142,#16143,#16144,#16145,#16146,
#16147,#16148,#16149,#16150,#16151,#16152,#16153,#16154,#16155,#16156,#16157,
#16158,#16159,#16160,#16161,#16162,#16163,#16164,#16165,#16166,#16167,#16168,
#16169,#16170,#16171,#16172,#16173,#16174)),.UNSPECIFIED.,.F.,.F.,.F.,(4,
4),(4,1,1,1,1,1,1,1,1,1,1,1,1,1,1,1,1,1,1,1,1,1,1,1,1,1,1,1,1,1,1,1,4),
(0.,0.0460148164544132),(11.6154215191107,12.6033609889557,13.5913004588008,
14.5792399286459,15.567179398491,16.5551188683361,17.5430583381812,18.5309978080262,
19.5189372778713,20.5068767477164,21.4948162175615,22.4827556874066,23.4706951572517,
24.4586346270967,25.4465740969418,26.4345135667869,27.422453036632,28.4103925064771,
29.3983319763222,30.3862714461672,31.3742109160123,32.3621503858574,33.3500898557025,
34.3380293255476,35.3259687953927,36.3139082652377,37.3018477350828,38.2897872049279,
39.277726674773,40.2656661446181,41.2536056144632,42.2415450843083,43.2294845541533),
 .UNSPECIFIED.);
#186=B_SPLINE_SURFACE_WITH_KNOTS('',3,3,((#17274,#17275,#17276,#17277,#17278,
#17279,#17280,#17281,#17282,#17283,#17284,#17285,#17286,#17287,#17288,#17289,
#17290,#17291,#17292,#17293,#17294,#17295,#17296,#17297,#17298,#17299,#17300,
#17301,#17302,#17303,#17304,#17305,#17306,#17307,#17308,#17309,#17310,#17311,
#17312,#17313,#17314,#17315,#17316,#17317,#17318,#17319,#17320,#17321,#17322,
#17323,#17324,#17325,#17326,#17327,#17328,#17329,#17330,#17331,#17332,#17333,
#17334,#17335,#17336,#17337,#17338,#17339,#17340,#17341,#17342,#17343,#17344,
#17345,#17346,#17347,#17348,#17349,#17350,#17351,#17352,#17353,#17354,#17355),
(#17356,#17357,#17358,#17359,#17360,#17361,#17362,#17363,#17364,#17365,
#17366,#17367,#17368,#17369,#17370,#17371,#17372,#17373,#17374,#17375,#17376,
#17377,#17378,#17379,#17380,#17381,#17382,#17383,#17384,#17385,#17386,#17387,
#17388,#17389,#17390,#17391,#17392,#17393,#17394,#17395,#17396,#17397,#17398,
#17399,#17400,#17401,#17402,#17403,#17404,#17405,#17406,#17407,#17408,#17409,
#17410,#17411,#17412,#17413,#17414,#17415,#17416,#17417,#17418,#17419,#17420,
#17421,#17422,#17423,#17424,#17425,#17426,#17427,#17428,#17429,#17430,#17431,
#17432,#17433,#17434,#17435,#17436,#17437),(#17438,#17439,#17440,#17441,
#17442,#17443,#17444,#17445,#17446,#17447,#17448,#17449,#17450,#17451,#17452,
#17453,#17454,#17455,#17456,#17457,#17458,#17459,#17460,#17461,#17462,#17463,
#17464,#17465,#17466,#17467,#17468,#17469,#17470,#17471,#17472,#17473,#17474,
#17475,#17476,#17477,#17478,#17479,#17480,#17481,#17482,#17483,#17484,#17485,
#17486,#17487,#17488,#17489,#17490,#17491,#17492,#17493,#17494,#17495,#17496,
#17497,#17498,#17499,#17500,#17501,#17502,#17503,#17504,#17505,#17506,#17507,
#17508,#17509,#17510,#17511,#17512,#17513,#17514,#17515,#17516,#17517,#17518,
#17519),(#17520,#17521,#17522,#17523,#17524,#17525,#17526,#17527,#17528,
#17529,#17530,#17531,#17532,#17533,#17534,#17535,#17536,#17537,#17538,#17539,
#17540,#17541,#17542,#17543,#17544,#17545,#17546,#17547,#17548,#17549,#17550,
#17551,#17552,#17553,#17554,#17555,#17556,#17557,#17558,#17559,#17560,#17561,
#17562,#17563,#17564,#17565,#17566,#17567,#17568,#17569,#17570,#17571,#17572,
#17573,#17574,#17575,#17576,#17577,#17578,#17579,#17580,#17581,#17582,#17583,
#17584,#17585,#17586,#17587,#17588,#17589,#17590,#17591,#17592,#17593,#17594,
#17595,#17596,#17597,#17598,#17599,#17600,#17601)),.UNSPECIFIED.,.F.,.F.,
 .F.,(4,4),(4,1,1,1,1,1,1,1,1,1,1,1,1,1,1,1,1,1,1,1,1,1,1,1,1,1,1,1,1,1,
1,1,1,1,1,1,1,1,1,1,1,1,1,1,1,1,1,1,1,1,1,1,1,1,1,1,1,1,1,1,1,1,1,1,1,1,
1,1,1,1,1,1,1,1,1,1,1,1,1,4),(0.,0.0329955678841871),(8.30203615430834,
9.29064014026014,10.2792441262119,11.2678481121638,12.2564520981156,13.2450560840674,
14.2336600700192,15.222264055971,16.2108680419228,17.1994720278746,18.1880760138264,
19.1766799997782,20.16528398573,21.1538879716818,22.1424919576336,23.1310959435854,
24.1196999295372,25.108303915489,26.0969079014409,27.0855118873927,28.0741158733445,
29.0627198592963,30.0513238452481,31.0399278311999,32.0285318171517,33.0171358031035,
34.0057397890553,34.9943437750071,35.9829477609589,36.9715517469107,37.9601557328625,
38.9487597188143,39.9373637047661,40.9259676907179,41.9145716766698,42.9031756626216,
43.8917796485734,44.8803836345252,45.868987620477,46.8575916064288,47.8461955923806,
48.8347995783324,49.8234035642842,50.812007550236,51.8006115361878,52.7892155221396,
53.7778195080914,54.7664234940432,55.755027479995,56.7436314659468,57.7322354518986,
58.7208394378505,59.7094434238023,60.6980474097541,61.6866513957059,62.6752553816577,
63.6638593676095,64.6524633535613,65.6410673395131,66.6296713254649,67.6182753114167,
68.6068792973685,69.5954832833203,70.5840872692721,71.5726912552239,72.5612952411758,
73.5498992271276,74.5385032130794,75.5271071990312,76.515711184983,77.5043151709348,
78.4929191568866,79.4815231428384,80.4701271287902,81.458731114742,82.4473351006938,
83.4359390866456,84.4245430725974,85.4131470585492,86.401751044501),
 .UNSPECIFIED.);
#187=B_SPLINE_SURFACE_WITH_KNOTS('',3,3,((#17813,#17814,#17815,#17816,#17817,
#17818,#17819,#17820,#17821,#17822,#17823,#17824,#17825,#17826,#17827,#17828,
#17829,#17830,#17831,#17832,#17833,#17834,#17835,#17836,#17837,#17838,#17839,
#17840,#17841,#17842,#17843,#17844,#17845,#17846,#17847,#17848,#17849,#17850,
#17851,#17852,#17853,#17854,#17855,#17856,#17857,#17858,#17859,#17860,#17861,
#17862,#17863,#17864,#17865,#17866,#17867,#17868,#17869,#17870,#17871,#17872,
#17873,#17874,#17875,#17876,#17877,#17878,#17879,#17880,#17881,#17882,#17883,
#17884,#17885,#17886,#17887,#17888,#17889,#17890,#17891,#17892,#17893,#17894),
(#17895,#17896,#17897,#17898,#17899,#17900,#17901,#17902,#17903,#17904,
#17905,#17906,#17907,#17908,#17909,#17910,#17911,#17912,#17913,#17914,#17915,
#17916,#17917,#17918,#17919,#17920,#17921,#17922,#17923,#17924,#17925,#17926,
#17927,#17928,#17929,#17930,#17931,#17932,#17933,#17934,#17935,#17936,#17937,
#17938,#17939,#17940,#17941,#17942,#17943,#17944,#17945,#17946,#17947,#17948,
#17949,#17950,#17951,#17952,#17953,#17954,#17955,#17956,#17957,#17958,#17959,
#17960,#17961,#17962,#17963,#17964,#17965,#17966,#17967,#17968,#17969,#17970,
#17971,#17972,#17973,#17974,#17975,#17976),(#17977,#17978,#17979,#17980,
#17981,#17982,#17983,#17984,#17985,#17986,#17987,#17988,#17989,#17990,#17991,
#17992,#17993,#17994,#17995,#17996,#17997,#17998,#17999,#18000,#18001,#18002,
#18003,#18004,#18005,#18006,#18007,#18008,#18009,#18010,#18011,#18012,#18013,
#18014,#18015,#18016,#18017,#18018,#18019,#18020,#18021,#18022,#18023,#18024,
#18025,#18026,#18027,#18028,#18029,#18030,#18031,#18032,#18033,#18034,#18035,
#18036,#18037,#18038,#18039,#18040,#18041,#18042,#18043,#18044,#18045,#18046,
#18047,#18048,#18049,#18050,#18051,#18052,#18053,#18054,#18055,#18056,#18057,
#18058),(#18059,#18060,#18061,#18062,#18063,#18064,#18065,#18066,#18067,
#18068,#18069,#18070,#18071,#18072,#18073,#18074,#18075,#18076,#18077,#18078,
#18079,#18080,#18081,#18082,#18083,#18084,#18085,#18086,#18087,#18088,#18089,
#18090,#18091,#18092,#18093,#18094,#18095,#18096,#18097,#18098,#18099,#18100,
#18101,#18102,#18103,#18104,#18105,#18106,#18107,#18108,#18109,#18110,#18111,
#18112,#18113,#18114,#18115,#18116,#18117,#18118,#18119,#18120,#18121,#18122,
#18123,#18124,#18125,#18126,#18127,#18128,#18129,#18130,#18131,#18132,#18133,
#18134,#18135,#18136,#18137,#18138,#18139,#18140)),.UNSPECIFIED.,.F.,.F.,
 .F.,(4,4),(4,1,1,1,1,1,1,1,1,1,1,1,1,1,1,1,1,1,1,1,1,1,1,1,1,1,1,1,1,1,
1,1,1,1,1,1,1,1,1,1,1,1,1,1,1,1,1,1,1,1,1,1,1,1,1,1,1,1,1,1,1,1,1,1,1,1,
1,1,1,1,1,1,1,1,1,1,1,1,1,4),(0.,0.0329955678841871),(11.6159397475004,
12.6045437334522,13.593147719404,14.5817517053558,15.5703556913076,16.5589596772594,
17.5475636632112,18.536167649163,19.5247716351148,20.5133756210666,21.5019796070184,
22.4905835929702,23.479187578922,24.4677915648739,25.4563955508257,26.4449995367775,
27.4336035227293,28.4222075086811,29.4108114946329,30.3994154805847,31.3880194665365,
32.3766234524883,33.3652274384401,34.3538314243919,35.3424354103437,36.3310393962955,
37.3196433822473,38.3082473681991,39.296851354151,40.2854553401028,41.2740593260546,
42.2626633120064,43.2512672979582,44.23987128391,45.2284752698618,46.2170792558136,
47.2056832417654,48.1942872277172,49.182891213669,50.1714951996208,51.1600991855726,
52.1487031715244,53.1373071574762,54.1259111434281,55.1145151293799,56.1031191153317,
57.0917231012835,58.0803270872353,59.0689310731871,60.0575350591389,61.0461390450907,
62.0347430310425,63.0233470169943,64.0119510029461,65.0005549888979,65.9891589748497,
66.9777629608015,67.9663669467533,68.9549709327052,69.943574918657,70.9321789046088,
71.9207828905606,72.9093868765124,73.8979908624642,74.886594848416,75.8751988343678,
76.8638028203196,77.8524068062714,78.8410107922232,79.829614778175,80.8182187641268,
81.8068227500786,82.7954267360304,83.7840307219822,84.7726347079341,85.7612386938859,
86.7498426798377,87.7384466657895,88.7270506517413,89.7156546376931),
 .UNSPECIFIED.);
#188=B_SPLINE_CURVE_WITH_KNOTS('',3,(#12551,#12552,#12553,#12554),
 .UNSPECIFIED.,.F.,.F.,(4,4),(-0.0416286806186443,-0.039090786429231),
 .UNSPECIFIED.);
#189=B_SPLINE_CURVE_WITH_KNOTS('',3,(#12563,#12564,#12565,#12566),
 .UNSPECIFIED.,.F.,.F.,(4,4),(-0.00358674747543116,-0.00105074276589837),
 .UNSPECIFIED.);
#190=B_SPLINE_CURVE_WITH_KNOTS('',3,(#12609,#12610,#12611,#12612,#12613,
#12614,#12615),.UNSPECIFIED.,.F.,.F.,(4,3,4),(0.,0.0165311745375961,0.035733654742842),
 .UNSPECIFIED.);
#191=B_SPLINE_CURVE_WITH_KNOTS('',3,(#12616,#12617,#12618,#12619,#12620,
#12621,#12622),.UNSPECIFIED.,.F.,.F.,(4,3,4),(0.093322390013544,0.111401256244007,
0.119257131462378),.UNSPECIFIED.);
#192=B_SPLINE_CURVE_WITH_KNOTS('',3,(#12625,#12626,#12627,#12628,#12629,
#12630,#12631),.UNSPECIFIED.,.F.,.F.,(4,3,4),(0.107846162587432,0.120934849613304,
0.1266096642358),.UNSPECIFIED.);
#193=B_SPLINE_CURVE_WITH_KNOTS('',3,(#12633,#12634,#12635,#12636),
 .UNSPECIFIED.,.F.,.F.,(4,4),(0.,0.0156100092084493),.UNSPECIFIED.);
#194=B_SPLINE_CURVE_WITH_KNOTS('',3,(#12653,#12654,#12655,#12656),
 .UNSPECIFIED.,.F.,.F.,(4,4),(-0.159704010702857,-0.0871316914258202),
 .UNSPECIFIED.);
#195=B_SPLINE_CURVE_WITH_KNOTS('',2,(#12658,#12659,#12660),
 .UNSPECIFIED.,.F.,.F.,(3,3),(0.626600308945203,1.),.UNSPECIFIED.);
#196=B_SPLINE_CURVE_WITH_KNOTS('',2,(#12664,#12665,#12666),
 .UNSPECIFIED.,.F.,.F.,(3,3),(0.930285828630975,1.),.UNSPECIFIED.);
#197=B_SPLINE_CURVE_WITH_KNOTS('',3,(#12667,#12668,#12669,#12670,#12671,
#12672,#12673),.UNSPECIFIED.,.F.,.F.,(4,3,4),(-0.0373027797814653,-0.0240644534710859,
0.),.UNSPECIFIED.);
#198=B_SPLINE_CURVE_WITH_KNOTS('',3,(#12676,#12677,#12678,#12679,#12680,
#12681,#12682,#12683,#12684,#12685),.UNSPECIFIED.,.F.,.F.,(4,3,3,4),(-0.19290526608905,
-0.149564698200622,-0.106837983631372,-0.0956446006455143),
 .UNSPECIFIED.);
#199=B_SPLINE_CURVE_WITH_KNOTS('',3,(#12699,#12700,#12701,#12702,#12703,
#12704,#12705,#12706,#12707,#12708),.UNSPECIFIED.,.F.,.F.,(4,2,2,2,4),(0.00995060155970214,
0.127861262644591,0.255722525289182,0.384625287958343,0.513528050627505),
 .UNSPECIFIED.);
#200=B_SPLINE_CURVE_WITH_KNOTS('',3,(#12743,#12744,#12745,#12746,#12747,
#12748,#12749,#12750,#12751,#12752),.UNSPECIFIED.,.F.,.F.,(4,2,2,2,4),(1.52050309692962,
1.64940585959878,1.77830862226794,1.90616988491253,2.02408054599742),
 .UNSPECIFIED.);
#201=B_SPLINE_CURVE_WITH_KNOTS('',3,(#12789,#12790,#12791,#12792,#12793,
#12794,#12795,#12796,#12797,#12798),.UNSPECIFIED.,.F.,.F.,(4,2,2,2,4),(0.518398684879072,
0.638089519791373,0.767732342509753,0.897375165228133,1.01706600014044),
 .UNSPECIFIED.);
#202=B_SPLINE_CURVE_WITH_KNOTS('',2,(#12813,#12814,#12815),
 .UNSPECIFIED.,.F.,.F.,(3,3),(0.,1.),.UNSPECIFIED.);
#203=B_SPLINE_CURVE_WITH_KNOTS('',2,(#12817,#12818,#12819),
 .UNSPECIFIED.,.F.,.F.,(3,3),(0.,1.),.UNSPECIFIED.);
#204=B_SPLINE_CURVE_WITH_KNOTS('',2,(#12821,#12822,#12823),
 .UNSPECIFIED.,.F.,.F.,(3,3),(0.,1.),.UNSPECIFIED.);
#205=B_SPLINE_CURVE_WITH_KNOTS('',2,(#12825,#12826,#12827),
 .UNSPECIFIED.,.F.,.F.,(3,3),(0.,1.),.UNSPECIFIED.);
#206=B_SPLINE_CURVE_WITH_KNOTS('',2,(#12829,#12830,#12831),
 .UNSPECIFIED.,.F.,.F.,(3,3),(0.,1.),.UNSPECIFIED.);
#207=B_SPLINE_CURVE_WITH_KNOTS('',2,(#12832,#12833,#12834),
 .UNSPECIFIED.,.F.,.F.,(3,3),(0.,0.31406597767443),.UNSPECIFIED.);
#208=B_SPLINE_CURVE_WITH_KNOTS('',2,(#12906,#12907,#12908),
 .UNSPECIFIED.,.F.,.F.,(3,3),(0.,1.),.UNSPECIFIED.);
#209=B_SPLINE_CURVE_WITH_KNOTS('',2,(#12910,#12911,#12912),
 .UNSPECIFIED.,.F.,.F.,(3,3),(0.,1.),.UNSPECIFIED.);
#210=B_SPLINE_CURVE_WITH_KNOTS('',2,(#12914,#12915,#12916),
 .UNSPECIFIED.,.F.,.F.,(3,3),(0.,1.),.UNSPECIFIED.);
#211=B_SPLINE_CURVE_WITH_KNOTS('',2,(#12918,#12919,#12920),
 .UNSPECIFIED.,.F.,.F.,(3,3),(0.,1.),.UNSPECIFIED.);
#212=B_SPLINE_CURVE_WITH_KNOTS('',2,(#12922,#12923,#12924),
 .UNSPECIFIED.,.F.,.F.,(3,3),(0.,1.),.UNSPECIFIED.);
#213=B_SPLINE_CURVE_WITH_KNOTS('',2,(#12926,#12927,#12928),
 .UNSPECIFIED.,.F.,.F.,(3,3),(0.,1.),.UNSPECIFIED.);
#214=B_SPLINE_CURVE_WITH_KNOTS('',2,(#12930,#12931,#12932),
 .UNSPECIFIED.,.F.,.F.,(3,3),(0.,1.),.UNSPECIFIED.);
#215=B_SPLINE_CURVE_WITH_KNOTS('',2,(#12934,#12935,#12936),
 .UNSPECIFIED.,.F.,.F.,(3,3),(0.,1.),.UNSPECIFIED.);
#216=B_SPLINE_CURVE_WITH_KNOTS('',2,(#12938,#12939,#12940),
 .UNSPECIFIED.,.F.,.F.,(3,3),(0.,1.),.UNSPECIFIED.);
#217=B_SPLINE_CURVE_WITH_KNOTS('',2,(#12942,#12943,#12944),
 .UNSPECIFIED.,.F.,.F.,(3,3),(0.,1.),.UNSPECIFIED.);
#218=B_SPLINE_CURVE_WITH_KNOTS('',2,(#12945,#12946,#12947),
 .UNSPECIFIED.,.F.,.F.,(3,3),(0.,1.),.UNSPECIFIED.);
#219=B_SPLINE_CURVE_WITH_KNOTS('',2,(#12970,#12971,#12972),
 .UNSPECIFIED.,.F.,.F.,(3,3),(0.,1.),.UNSPECIFIED.);
#220=B_SPLINE_CURVE_WITH_KNOTS('',2,(#12974,#12975,#12976),
 .UNSPECIFIED.,.F.,.F.,(3,3),(0.,1.),.UNSPECIFIED.);
#221=B_SPLINE_CURVE_WITH_KNOTS('',2,(#12978,#12979,#12980),
 .UNSPECIFIED.,.F.,.F.,(3,3),(0.,1.),.UNSPECIFIED.);
#222=B_SPLINE_CURVE_WITH_KNOTS('',2,(#12982,#12983,#12984),
 .UNSPECIFIED.,.F.,.F.,(3,3),(0.,1.),.UNSPECIFIED.);
#223=B_SPLINE_CURVE_WITH_KNOTS('',2,(#12986,#12987,#12988),
 .UNSPECIFIED.,.F.,.F.,(3,3),(0.,1.),.UNSPECIFIED.);
#224=B_SPLINE_CURVE_WITH_KNOTS('',2,(#12990,#12991,#12992),
 .UNSPECIFIED.,.F.,.F.,(3,3),(0.,1.),.UNSPECIFIED.);
#225=B_SPLINE_CURVE_WITH_KNOTS('',2,(#12994,#12995,#12996),
 .UNSPECIFIED.,.F.,.F.,(3,3),(0.,1.),.UNSPECIFIED.);
#226=B_SPLINE_CURVE_WITH_KNOTS('',2,(#12998,#12999,#13000),
 .UNSPECIFIED.,.F.,.F.,(3,3),(0.,1.),.UNSPECIFIED.);
#227=B_SPLINE_CURVE_WITH_KNOTS('',2,(#13002,#13003,#13004),
 .UNSPECIFIED.,.F.,.F.,(3,3),(0.,1.),.UNSPECIFIED.);
#228=B_SPLINE_CURVE_WITH_KNOTS('',2,(#13006,#13007,#13008),
 .UNSPECIFIED.,.F.,.F.,(3,3),(0.,1.),.UNSPECIFIED.);
#229=B_SPLINE_CURVE_WITH_KNOTS('',2,(#13009,#13010,#13011),
 .UNSPECIFIED.,.F.,.F.,(3,3),(0.,1.),.UNSPECIFIED.);
#230=B_SPLINE_CURVE_WITH_KNOTS('',2,(#13016,#13017,#13018),
 .UNSPECIFIED.,.F.,.F.,(3,3),(0.,1.),.UNSPECIFIED.);
#231=B_SPLINE_CURVE_WITH_KNOTS('',2,(#13020,#13021,#13022),
 .UNSPECIFIED.,.F.,.F.,(3,3),(0.,1.),.UNSPECIFIED.);
#232=B_SPLINE_CURVE_WITH_KNOTS('',2,(#13024,#13025,#13026),
 .UNSPECIFIED.,.F.,.F.,(3,3),(0.,1.),.UNSPECIFIED.);
#233=B_SPLINE_CURVE_WITH_KNOTS('',2,(#13028,#13029,#13030),
 .UNSPECIFIED.,.F.,.F.,(3,3),(0.,1.),.UNSPECIFIED.);
#234=B_SPLINE_CURVE_WITH_KNOTS('',2,(#13032,#13033,#13034),
 .UNSPECIFIED.,.F.,.F.,(3,3),(0.,1.),.UNSPECIFIED.);
#235=B_SPLINE_CURVE_WITH_KNOTS('',2,(#13036,#13037,#13038),
 .UNSPECIFIED.,.F.,.F.,(3,3),(0.,1.),.UNSPECIFIED.);
#236=B_SPLINE_CURVE_WITH_KNOTS('',2,(#13040,#13041,#13042),
 .UNSPECIFIED.,.F.,.F.,(3,3),(0.,1.),.UNSPECIFIED.);
#237=B_SPLINE_CURVE_WITH_KNOTS('',2,(#13044,#13045,#13046),
 .UNSPECIFIED.,.F.,.F.,(3,3),(0.,1.),.UNSPECIFIED.);
#238=B_SPLINE_CURVE_WITH_KNOTS('',2,(#13048,#13049,#13050),
 .UNSPECIFIED.,.F.,.F.,(3,3),(0.,1.),.UNSPECIFIED.);
#239=B_SPLINE_CURVE_WITH_KNOTS('',2,(#13052,#13053,#13054),
 .UNSPECIFIED.,.F.,.F.,(3,3),(0.,1.),.UNSPECIFIED.);
#240=B_SPLINE_CURVE_WITH_KNOTS('',2,(#13055,#13056,#13057),
 .UNSPECIFIED.,.F.,.F.,(3,3),(0.,1.),.UNSPECIFIED.);
#241=B_SPLINE_CURVE_WITH_KNOTS('',3,(#13091,#13092,#13093,#13094,#13095,
#13096,#13097,#13098,#13099,#13100),.UNSPECIFIED.,.F.,.F.,(4,2,2,2,4),(1.01688813186998,
1.13657896678228,1.26622178950066,1.39586461221904,1.51555544713135),
 .UNSPECIFIED.);
#242=B_SPLINE_CURVE_WITH_KNOTS('',2,(#13149,#13150,#13151),
 .UNSPECIFIED.,.F.,.F.,(3,3),(0.,0.369411589751801),.UNSPECIFIED.);
#243=B_SPLINE_CURVE_WITH_KNOTS('',2,(#13153,#13154,#13155),
 .UNSPECIFIED.,.F.,.F.,(3,3),(0.,1.),.UNSPECIFIED.);
#244=B_SPLINE_CURVE_WITH_KNOTS('',2,(#13157,#13158,#13159),
 .UNSPECIFIED.,.F.,.F.,(3,3),(0.,1.),.UNSPECIFIED.);
#245=B_SPLINE_CURVE_WITH_KNOTS('',2,(#13161,#13162,#13163),
 .UNSPECIFIED.,.F.,.F.,(3,3),(0.,1.),.UNSPECIFIED.);
#246=B_SPLINE_CURVE_WITH_KNOTS('',2,(#13165,#13166,#13167),
 .UNSPECIFIED.,.F.,.F.,(3,3),(0.,1.),.UNSPECIFIED.);
#247=B_SPLINE_CURVE_WITH_KNOTS('',2,(#13168,#13169,#13170),
 .UNSPECIFIED.,.F.,.F.,(3,3),(0.,1.),.UNSPECIFIED.);
#248=B_SPLINE_CURVE_WITH_KNOTS('',2,(#13365,#13366,#13367),
 .UNSPECIFIED.,.F.,.F.,(3,3),(0.,1.),.UNSPECIFIED.);
#249=B_SPLINE_CURVE_WITH_KNOTS('',2,(#13377,#13378,#13379),
 .UNSPECIFIED.,.F.,.F.,(3,3),(0.,1.),.UNSPECIFIED.);
#250=B_SPLINE_CURVE_WITH_KNOTS('',2,(#13388,#13389,#13390),
 .UNSPECIFIED.,.F.,.F.,(3,3),(0.,1.),.UNSPECIFIED.);
#251=B_SPLINE_CURVE_WITH_KNOTS('',2,(#13399,#13400,#13401),
 .UNSPECIFIED.,.F.,.F.,(3,3),(0.,1.),.UNSPECIFIED.);
#252=B_SPLINE_CURVE_WITH_KNOTS('',2,(#13410,#13411,#13412),
 .UNSPECIFIED.,.F.,.F.,(3,3),(0.,1.),.UNSPECIFIED.);
#253=B_SPLINE_CURVE_WITH_KNOTS('',2,(#13421,#13422,#13423),
 .UNSPECIFIED.,.F.,.F.,(3,3),(0.,1.),.UNSPECIFIED.);
#254=B_SPLINE_CURVE_WITH_KNOTS('',2,(#13432,#13433,#13434),
 .UNSPECIFIED.,.F.,.F.,(3,3),(0.,1.),.UNSPECIFIED.);
#255=B_SPLINE_CURVE_WITH_KNOTS('',2,(#13443,#13444,#13445),
 .UNSPECIFIED.,.F.,.F.,(3,3),(0.,1.),.UNSPECIFIED.);
#256=B_SPLINE_CURVE_WITH_KNOTS('',2,(#13454,#13455,#13456),
 .UNSPECIFIED.,.F.,.F.,(3,3),(0.,1.),.UNSPECIFIED.);
#257=B_SPLINE_CURVE_WITH_KNOTS('',2,(#13465,#13466,#13467),
 .UNSPECIFIED.,.F.,.F.,(3,3),(0.,1.),.UNSPECIFIED.);
#258=B_SPLINE_CURVE_WITH_KNOTS('',2,(#13474,#13475,#13476),
 .UNSPECIFIED.,.F.,.F.,(3,3),(0.,1.),.UNSPECIFIED.);
#259=B_SPLINE_CURVE_WITH_KNOTS('',2,(#13528,#13529,#13530),
 .UNSPECIFIED.,.F.,.F.,(3,3),(0.,1.),.UNSPECIFIED.);
#260=B_SPLINE_CURVE_WITH_KNOTS('',2,(#13540,#13541,#13542),
 .UNSPECIFIED.,.F.,.F.,(3,3),(0.,1.),.UNSPECIFIED.);
#261=B_SPLINE_CURVE_WITH_KNOTS('',2,(#13551,#13552,#13553),
 .UNSPECIFIED.,.F.,.F.,(3,3),(0.,1.),.UNSPECIFIED.);
#262=B_SPLINE_CURVE_WITH_KNOTS('',2,(#13562,#13563,#13564),
 .UNSPECIFIED.,.F.,.F.,(3,3),(0.,1.),.UNSPECIFIED.);
#263=B_SPLINE_CURVE_WITH_KNOTS('',2,(#13573,#13574,#13575),
 .UNSPECIFIED.,.F.,.F.,(3,3),(0.,1.),.UNSPECIFIED.);
#264=B_SPLINE_CURVE_WITH_KNOTS('',2,(#13584,#13585,#13586),
 .UNSPECIFIED.,.F.,.F.,(3,3),(0.,1.),.UNSPECIFIED.);
#265=B_SPLINE_CURVE_WITH_KNOTS('',2,(#13595,#13596,#13597),
 .UNSPECIFIED.,.F.,.F.,(3,3),(0.,1.),.UNSPECIFIED.);
#266=B_SPLINE_CURVE_WITH_KNOTS('',2,(#13606,#13607,#13608),
 .UNSPECIFIED.,.F.,.F.,(3,3),(0.,1.),.UNSPECIFIED.);
#267=B_SPLINE_CURVE_WITH_KNOTS('',2,(#13617,#13618,#13619),
 .UNSPECIFIED.,.F.,.F.,(3,3),(0.,1.),.UNSPECIFIED.);
#268=B_SPLINE_CURVE_WITH_KNOTS('',2,(#13628,#13629,#13630),
 .UNSPECIFIED.,.F.,.F.,(3,3),(0.,1.),.UNSPECIFIED.);
#269=B_SPLINE_CURVE_WITH_KNOTS('',2,(#13637,#13638,#13639),
 .UNSPECIFIED.,.F.,.F.,(3,3),(0.,1.),.UNSPECIFIED.);
#270=B_SPLINE_CURVE_WITH_KNOTS('',2,(#13691,#13692,#13693),
 .UNSPECIFIED.,.F.,.F.,(3,3),(0.,1.),.UNSPECIFIED.);
#271=B_SPLINE_CURVE_WITH_KNOTS('',2,(#13703,#13704,#13705),
 .UNSPECIFIED.,.F.,.F.,(3,3),(0.,1.),.UNSPECIFIED.);
#272=B_SPLINE_CURVE_WITH_KNOTS('',2,(#13714,#13715,#13716),
 .UNSPECIFIED.,.F.,.F.,(3,3),(0.,1.),.UNSPECIFIED.);
#273=B_SPLINE_CURVE_WITH_KNOTS('',2,(#13725,#13726,#13727),
 .UNSPECIFIED.,.F.,.F.,(3,3),(0.,1.),.UNSPECIFIED.);
#274=B_SPLINE_CURVE_WITH_KNOTS('',2,(#13736,#13737,#13738),
 .UNSPECIFIED.,.F.,.F.,(3,3),(0.,1.),.UNSPECIFIED.);
#275=B_SPLINE_CURVE_WITH_KNOTS('',2,(#13747,#13748,#13749),
 .UNSPECIFIED.,.F.,.F.,(3,3),(0.,1.),.UNSPECIFIED.);
#276=B_SPLINE_CURVE_WITH_KNOTS('',2,(#13758,#13759,#13760),
 .UNSPECIFIED.,.F.,.F.,(3,3),(0.,1.),.UNSPECIFIED.);
#277=B_SPLINE_CURVE_WITH_KNOTS('',2,(#13769,#13770,#13771),
 .UNSPECIFIED.,.F.,.F.,(3,3),(0.,1.),.UNSPECIFIED.);
#278=B_SPLINE_CURVE_WITH_KNOTS('',2,(#13780,#13781,#13782),
 .UNSPECIFIED.,.F.,.F.,(3,3),(0.,1.),.UNSPECIFIED.);
#279=B_SPLINE_CURVE_WITH_KNOTS('',2,(#13791,#13792,#13793),
 .UNSPECIFIED.,.F.,.F.,(3,3),(0.,1.),.UNSPECIFIED.);
#280=B_SPLINE_CURVE_WITH_KNOTS('',2,(#13800,#13801,#13802),
 .UNSPECIFIED.,.F.,.F.,(3,3),(0.,1.),.UNSPECIFIED.);
#281=B_SPLINE_CURVE_WITH_KNOTS('',3,(#14708,#14709,#14710,#14711,#14712,
#14713,#14714,#14715,#14716,#14717,#14718,#14719,#14720,#14721,#14722,#14723,
#14724,#14725,#14726,#14727),.UNSPECIFIED.,.T.,.F.,(4,1,1,1,1,1,1,1,1,1,
1,1,1,1,1,1,1,4),(0.929489890414013,1.01801273712011,1.06227416047316,1.10653558382621,
1.1950584305323,1.2835812772384,1.3721041239445,1.41636554729754,1.46062697065059,
1.54914981735669,1.63767266406279,1.68193408741583,1.72619551076888,1.81471835747498,
1.90324120418107,1.99176405088717,2.08028689759327,2.16880974429936),
 .UNSPECIFIED.);
#282=B_SPLINE_CURVE_WITH_KNOTS('',3,(#14728,#14729,#14730,#14731,#14732,
#14733,#14734,#14735,#14736,#14737,#14738,#14739,#14740,#14741,#14742,#14743,
#14744,#14745,#14746,#14747),.UNSPECIFIED.,.T.,.F.,(4,1,1,1,1,1,1,1,1,1,
1,1,1,1,1,1,1,4),(-2.16880974429936,-2.08028689759327,-1.99176405088717,
-1.90324120418107,-1.81471835747498,-1.72619551076888,-1.68193408741583,
-1.63767266406279,-1.54914981735669,-1.46062697065059,-1.41636554729754,
-1.3721041239445,-1.2835812772384,-1.1950584305323,-1.10653558382621,-1.06227416047316,
-1.01801273712011,-0.929489890414013),.UNSPECIFIED.);
#283=B_SPLINE_CURVE_WITH_KNOTS('',3,(#14752,#14753,#14754,#14755,#14756,
#14757,#14758,#14759,#14760,#14761),.UNSPECIFIED.,.F.,.F.,(4,2,2,2,4),(0.,
0.0782650235733475,0.156530047146695,0.234708817404274,0.312887587661852),
 .UNSPECIFIED.);
#284=B_SPLINE_CURVE_WITH_KNOTS('',3,(#14762,#14763,#14764,#14765,#14766,
#14767,#14768,#14769,#14770,#14771,#14772,#14773,#14774,#14775,#14776,#14777,
#14778,#14779,#14780,#14781,#14782,#14783,#14784,#14785,#14786,#14787),
 .UNSPECIFIED.,.F.,.F.,(4,2,2,2,2,2,2,2,2,2,2,2,4),(0.312887587661852,0.391066357919431,
0.469245128177009,0.547510151750357,0.625775175323705,0.704040198897052,
0.782305222470399,0.860483992727978,0.938662762985557,1.01684153324314,
1.09502030350071,1.17328532707406,1.25155035064741),.UNSPECIFIED.);
#285=B_SPLINE_CURVE_WITH_KNOTS('',3,(#15173,#15174,#15175,#15176,#15177,
#15178,#15179,#15180,#15181,#15182),.UNSPECIFIED.,.F.,.F.,(4,3,3,4),(-4.09254174883831,
-3.95175787938034,-2.96381840953525,-2.0651401332781),.UNSPECIFIED.);
#286=B_SPLINE_CURVE_WITH_KNOTS('',3,(#15185,#15186,#15187,#15188,#15189,
#15190,#15191),.UNSPECIFIED.,.F.,.F.,(4,3,4),(0.,0.987939469845084,1.11419103802959),
 .UNSPECIFIED.);
#287=B_SPLINE_CURVE_WITH_KNOTS('',3,(#15196,#15197,#15198,#15199,#15200,
#15201,#15202,#15203,#15204,#15205,#15206,#15207,#15208,#15209,#15210,#15211,
#15212,#15213,#15214,#15215,#15216,#15217),.UNSPECIFIED.,.F.,.F.,(4,3,3,
3,3,3,3,4),(-10.3757270560179,-9.87939469845084,-8.89145522860576,-7.90351575876067,
-6.91557628891559,-5.92763681907051,-4.93969734922542,-4.09254174883831),
 .UNSPECIFIED.);
#288=B_SPLINE_CURVE_WITH_KNOTS('',3,(#15218,#15219,#15220,#15221,#15222,
#15223,#15224,#15225,#15226,#15227,#15228,#15229,#15230,#15231,#15232,#15233,
#15234,#15235,#15236,#15237,#15238,#15239),.UNSPECIFIED.,.F.,.F.,(4,3,3,
3,3,3,3,4),(1.11419103802959,1.97587893969017,2.96381840953525,3.95175787938034,
4.93969734922542,5.9276368190705,6.91557628891559,7.39737634520918),
 .UNSPECIFIED.);
#289=B_SPLINE_CURVE_WITH_KNOTS('',3,(#15244,#15245,#15246,#15247,#15248,
#15249,#15250,#15251,#15252,#15253,#15254,#15255,#15256,#15257,#15258,#15259,
#15260,#15261,#15262,#15263,#15264,#15265),.UNSPECIFIED.,.F.,.F.,(4,3,3,
3,3,3,3,4),(-16.6589123631975,-15.8070315175213,-14.8190920476763,-13.8311525778312,
-12.8432131079861,-11.855273638141,-10.8673341682959,-10.3757270560179),
 .UNSPECIFIED.);
#290=B_SPLINE_CURVE_WITH_KNOTS('',3,(#15266,#15267,#15268,#15269,#15270,
#15271,#15272,#15273,#15274,#15275,#15276,#15277,#15278,#15279,#15280,#15281,
#15282,#15283,#15284,#15285,#15286,#15287),.UNSPECIFIED.,.F.,.F.,(4,3,3,
3,3,3,3,4),(7.39737634520918,7.90351575876067,8.89145522860576,9.87939469845084,
10.8673341682959,11.855273638141,12.8432131079861,13.6805616523888),
 .UNSPECIFIED.);
#291=B_SPLINE_CURVE_WITH_KNOTS('',3,(#15292,#15293,#15294,#15295,#15296,
#15297,#15298,#15299,#15300,#15301,#15302,#15303,#15304,#15305,#15306,#15307,
#15308,#15309,#15310,#15311,#15312,#15313,#15314,#15315,#15316),
 .UNSPECIFIED.,.F.,.F.,(4,3,3,3,3,3,3,3,4),(-22.9420976703771,-22.7226078064369,
-21.7346683365918,-20.7467288667468,-19.7587893969017,-18.7708499270566,
-17.7829104572115,-16.7949709873664,-16.6589123631975),.UNSPECIFIED.);
#292=B_SPLINE_CURVE_WITH_KNOTS('',3,(#15317,#15318,#15319,#15320,#15321,
#15322,#15323,#15324,#15325,#15326,#15327,#15328,#15329,#15330,#15331,#15332,
#15333,#15334,#15335,#15336,#15337,#15338,#15339,#15340,#15341),
 .UNSPECIFIED.,.F.,.F.,(4,3,3,3,3,3,3,3,4),(13.6805616523888,13.8311525778312,
14.8190920476763,15.8070315175213,16.7949709873664,17.7829104572115,18.7708499270566,
19.7587893969017,19.9637469595684),.UNSPECIFIED.);
#293=B_SPLINE_CURVE_WITH_KNOTS('',3,(#15346,#15347,#15348,#15349,#15350,
#15351,#15352,#15353,#15354,#15355,#15356,#15357,#15358,#15359,#15360,#15361,
#15362,#15363,#15364,#15365,#15366,#15367),.UNSPECIFIED.,.F.,.F.,(4,3,3,
3,3,3,3,4),(-29.2252829775566,-28.6502446255074,-27.6623051556623,-26.6743656858173,
-25.6864262159722,-24.6984867461271,-23.710547276282,-22.9420976703771),
 .UNSPECIFIED.);
#294=B_SPLINE_CURVE_WITH_KNOTS('',3,(#15368,#15369,#15370,#15371,#15372,
#15373,#15374,#15375,#15376,#15377,#15378,#15379,#15380,#15381,#15382,#15383,
#15384,#15385,#15386,#15387,#15388,#15389),.UNSPECIFIED.,.F.,.F.,(4,3,3,
3,3,3,3,4),(19.9637469595684,20.7467288667468,21.7346683365918,22.7226078064369,
23.710547276282,24.6984867461271,25.6864262159722,26.2469322667479),
 .UNSPECIFIED.);
#295=B_SPLINE_CURVE_WITH_KNOTS('',3,(#15395,#15396,#15397,#15398),
 .UNSPECIFIED.,.F.,.F.,(4,4),(40.8407044966673,41.1643444208752),
 .UNSPECIFIED.);
#296=B_SPLINE_CURVE_WITH_KNOTS('',3,(#15404,#15405,#15406,#15407,#15408,
#15409,#15410,#15411,#15412,#15413),.UNSPECIFIED.,.F.,.F.,(4,1,1,1,1,1,
1,4),(34.5575191894877,35.3259687953927,36.3139082652377,37.3018477350828,
38.2897872049279,39.277726674773,40.2656661446181,40.8407044966673),
 .UNSPECIFIED.);
#297=B_SPLINE_CURVE_WITH_KNOTS('',3,(#15416,#15417,#15418,#15419,#15420,
#15421,#15422,#15423,#15424),.UNSPECIFIED.,.F.,.F.,(4,1,1,1,1,1,4),(34.5575191894877,
34.9849526085571,35.9728920784021,36.9608315482472,37.9487710180923,38.9367104879374,
39.9246499577825),.UNSPECIFIED.);
#298=B_SPLINE_CURVE_WITH_KNOTS('',3,(#15429,#15430,#15431,#15432,#15433,
#15434,#15435,#15436,#15437,#15438,#15439),.UNSPECIFIED.,.F.,.F.,(4,1,1,
1,1,1,1,1,4),(28.2743338823081,28.4103925064771,29.3983319763222,30.3862714461672,
31.3742109160123,32.3621503858574,33.3500898557025,34.3380293255476,34.5575191894877),
 .UNSPECIFIED.);
#299=B_SPLINE_CURVE_WITH_KNOTS('',3,(#15440,#15441,#15442,#15443,#15444,
#15445,#15446,#15447,#15448,#15449),.UNSPECIFIED.,.F.,.F.,(4,1,1,1,1,1,
1,4),(28.2743338823081,29.0573157894865,30.0452552593316,31.0331947291767,
32.0211341990218,33.0090736688669,33.997013138712,34.5575191894877),
 .UNSPECIFIED.);
#300=B_SPLINE_CURVE_WITH_KNOTS('',3,(#15454,#15455,#15456,#15457,#15458,
#15459,#15460,#15461,#15462,#15463),.UNSPECIFIED.,.F.,.F.,(4,1,1,1,1,1,
1,4),(21.9911485751286,22.4827556874066,23.4706951572517,24.4586346270967,
25.4465740969418,26.4345135667869,27.422453036632,28.2743338823081),
 .UNSPECIFIED.);
#301=B_SPLINE_CURVE_WITH_KNOTS('',3,(#15464,#15465,#15466,#15467,#15468,
#15469,#15470,#15471,#15472,#15473,#15474),.UNSPECIFIED.,.F.,.F.,(4,1,1,
1,1,1,1,1,4),(21.9911485751285,22.141739500571,23.129678970416,24.1176184402611,
25.1055579101062,26.0934973799513,27.0814368497964,28.0693763196415,28.2743338823081),
 .UNSPECIFIED.);
#302=B_SPLINE_CURVE_WITH_KNOTS('',3,(#15479,#15480,#15481,#15482,#15483,
#15484,#15485,#15486,#15487,#15488),.UNSPECIFIED.,.F.,.F.,(4,1,1,1,1,1,
1,4),(15.707963267949,16.5551188683361,17.5430583381812,18.5309978080262,
19.5189372778713,20.5068767477164,21.4948162175615,21.9911485751286),
 .UNSPECIFIED.);
#303=B_SPLINE_CURVE_WITH_KNOTS('',3,(#15489,#15490,#15491,#15492,#15493,
#15494,#15495,#15496,#15497,#15498),.UNSPECIFIED.,.F.,.F.,(4,1,1,1,1,1,
1,4),(15.707963267949,16.2141026815005,17.2020421513455,18.1899816211906,
19.1779210910357,20.1658605608808,21.1538000307259,21.9911485751285),
 .UNSPECIFIED.);
#304=B_SPLINE_CURVE_WITH_KNOTS('',3,(#15501,#15502,#15503,#15504,#15505,
#15506,#15507,#15508,#15509,#15510,#15511,#15512,#15513,#15514,#15515,#15516,
#15517,#15518,#15519,#15520,#15521,#15522,#15523,#15524,#15525,#15526,#15527,
#15528,#15529,#15530,#15531,#15532,#15533,#15534,#15535,#15536,#15537,#15538,
#15539,#15540,#15541,#15542,#15543,#15544,#15545,#15546,#15547,#15548,#15549,
#15550,#15551,#15552,#15553,#15554,#15555,#15556,#15557,#15558,#15559,#15560,
#15561,#15562,#15563,#15564,#15565,#15566,#15567,#15568,#15569,#15570,#15571,
#15572,#15573,#15574,#15575,#15576,#15577,#15578,#15579,#15580,#15581,#15582,
#15583,#15584,#15585,#15586,#15587,#15588),.UNSPECIFIED.,.F.,.F.,(4,3,3,
3,3,3,3,3,3,3,3,3,3,3,3,3,3,3,3,3,3,3,3,3,3,3,3,3,3,4),(-0.366397579005854,
-0.352255736410487,-0.334218451541838,-0.328253122886177,-0.324086270819476,
-0.305360245801884,-0.290366742965128,-0.282186410845882,-0.278570970941181,
-0.259174525664227,-0.239360492094141,-0.225873424847565,-0.218279744579071,
-0.21479349407462,-0.194366185320955,-0.185412223107839,-0.1656728542356,
-0.155318300845875,-0.149835977262723,-0.146387185330202,-0.142989257238056,
-0.122499062045188,-0.10158515832526,-0.0805240629991821,-0.0758041242659399,
-0.0722178501685304,-0.050582110738417,-0.0288905415059291,-0.00765380511821571,
0.),.UNSPECIFIED.);
#305=B_SPLINE_CURVE_WITH_KNOTS('',3,(#15593,#15594,#15595,#15596,#15597,
#15598,#15599,#15600,#15601,#15602,#15603,#15604,#15605,#15606,#15607,#15608,
#15609,#15610,#15611,#15612,#15613,#15614,#15615,#15616,#15617,#15618,#15619,
#15620,#15621,#15622,#15623,#15624,#15625,#15626,#15627,#15628,#15629,#15630,
#15631,#15632,#15633,#15634,#15635,#15636,#15637,#15638,#15639,#15640,#15641,
#15642,#15643,#15644,#15645,#15646,#15647,#15648,#15649,#15650,#15651,#15652,
#15653,#15654,#15655,#15656,#15657,#15658,#15659,#15660,#15661,#15662,#15663,
#15664,#15665,#15666,#15667,#15668,#15669,#15670,#15671,#15672,#15673,#15674,
#15675,#15676,#15677,#15678,#15679,#15680),.UNSPECIFIED.,.F.,.F.,(4,3,3,
3,3,3,3,3,3,3,3,3,3,3,3,3,3,3,3,3,3,3,3,3,3,3,3,3,3,4),(-0.364629307890676,
-0.347233186800937,-0.325605321922639,-0.318094543245741,-0.313657346060215,
-0.309559480087559,-0.288242603902967,-0.272777082256873,-0.267225305920237,
-0.263420566366538,-0.24268211184628,-0.222383830675501,-0.20791748069018,
-0.196986121529868,-0.193341724847835,-0.17372888638403,-0.164518430734214,
-0.144479075481155,-0.134892353717832,-0.129096949286913,-0.12579032958573,
-0.106361418226009,-0.0869541719015021,-0.0679077912466892,-0.0628545069907101,
-0.0595313101688987,-0.0409300680615467,-0.0226566529034227,-0.00496781908450919,
0.),.UNSPECIFIED.);
#306=B_SPLINE_CURVE_WITH_KNOTS('',3,(#15821,#15822,#15823,#15824,#15825,
#15826,#15827,#15828,#15829,#15830,#15831,#15832,#15833),.UNSPECIFIED.,
 .F.,.F.,(4,3,3,3,4),(26.2469322667479,26.6743656858173,27.6623051556624,
28.6502446255074,29.5489229017646),.UNSPECIFIED.);
#307=B_SPLINE_CURVE_WITH_KNOTS('',3,(#15835,#15836,#15837,#15838,#15839,
#15840,#15841,#15842,#15843,#15844,#15845,#15846,#15847,#15848,#15849,#15850,
#15851,#15852,#15853,#15854,#15855,#15856,#15857,#15858,#15859,#15860,#15861,
#15862,#15863,#15864,#15865,#15866,#15867,#15868,#15869,#15870,#15871,#15872,
#15873,#15874,#15875,#15876,#15877,#15878,#15879,#15880,#15881,#15882,#15883,
#15884,#15885,#15886,#15887,#15888,#15889,#15890,#15891,#15892,#15893,#15894,
#15895,#15896,#15897,#15898,#15899,#15900,#15901,#15902,#15903,#15904,#15905,
#15906,#15907,#15908,#15909,#15910,#15911,#15912,#15913,#15914,#15915,#15916,
#15917,#15918,#15919,#15920,#15921,#15922),.UNSPECIFIED.,.F.,.F.,(4,3,3,
3,3,3,3,3,3,3,3,3,3,3,3,3,3,3,3,3,3,3,3,3,3,3,3,3,3,4),(-0.366397579005844,
-0.352255736410479,-0.334218432653028,-0.328253038170767,-0.324086234565793,
-0.305360194129425,-0.290366697751727,-0.282186333509408,-0.278570909684785,
-0.259174452080044,-0.239360419305942,-0.225873370256417,-0.218279602851231,
-0.214793320223163,-0.194366011802257,-0.185412223107841,-0.165672847130201,
-0.155318294184563,-0.149835975114951,-0.146387182322352,-0.142989257864255,
-0.122499054249301,-0.101585142121661,-0.0805240463756091,-0.0758040661415852,
-0.0722178274121236,-0.0505820817915926,-0.0288905167825514,-0.00765380478964332,
0.),.UNSPECIFIED.);
#308=B_SPLINE_CURVE_WITH_KNOTS('',3,(#15923,#15924,#15925,#15926,#15927,
#15928,#15929,#15930,#15931),.UNSPECIFIED.,.F.,.F.,(4,1,1,1,1,1,4),(10.3757270560179,
11.274405332275,12.2623448021201,13.2502842719652,14.2382237418103,15.2261632116554,
15.707963267949),.UNSPECIFIED.);
#309=B_SPLINE_CURVE_WITH_KNOTS('',3,(#15937,#15938,#15939,#15940,#15941,
#15942,#15943,#15944,#15945,#15946,#15947,#15948,#15949,#15950,#15951,#15952,
#15953,#15954,#15955,#15956,#15957,#15958,#15959,#15960,#15961,#15962,#15963,
#15964,#15965,#15966,#15967,#15968,#15969,#15970,#15971,#15972,#15973,#15974,
#15975,#15976,#15977,#15978,#15979,#15980,#15981,#15982,#15983,#15984,#15985,
#15986,#15987,#15988,#15989,#15990,#15991,#15992,#15993,#15994,#15995,#15996,
#15997,#15998,#15999,#16000,#16001,#16002,#16003,#16004,#16005,#16006,#16007,
#16008,#16009,#16010,#16011,#16012,#16013,#16014,#16015,#16016,#16017,#16018,
#16019,#16020,#16021,#16022,#16023,#16024),.UNSPECIFIED.,.F.,.F.,(4,3,3,
3,3,3,3,3,3,3,3,3,3,3,3,3,3,3,3,3,3,3,3,3,3,3,3,3,3,4),(-0.364629307890668,
-0.347233186800931,-0.325605321836021,-0.318094550462088,-0.313657357457997,
-0.309559484803747,-0.288242609186508,-0.272777086879971,-0.267225319700862,
-0.263420582037393,-0.242682128922672,-0.222383863217287,-0.207917505096519,
-0.19698615658864,-0.193341780935945,-0.173728958311534,-0.164518430734215,
-0.144479084110425,-0.134892371590082,-0.129097020267292,-0.125790396614882,
-0.106361491905245,-0.0869542352211722,-0.0679078299359471,-0.0628545671260098,
-0.0595313315005194,-0.0409300719336087,-0.0226566308768889,-0.0049677658155539,
0.),.UNSPECIFIED.);
#310=B_SPLINE_CURVE_WITH_KNOTS('',3,(#16027,#16028,#16029,#16030,#16031,
#16032,#16033,#16034),.UNSPECIFIED.,.F.,.F.,(4,1,1,1,1,4),(11.6154215191107,
12.6033609889557,13.5913004588008,14.5792399286459,15.567179398491,15.707963267949),
 .UNSPECIFIED.);
#311=B_SPLINE_CURVE_WITH_KNOTS('',3,(#16175,#16176,#16177,#16178,#16179,
#16180,#16181,#16182,#16183,#16184),.UNSPECIFIED.,.F.,.F.,(4,3,3,4),(-31.6140630350427,
-30.6261235651976,-29.6381840953525,-29.2252829775566),.UNSPECIFIED.);
#312=B_SPLINE_CURVE_WITH_KNOTS('',3,(#16240,#16241,#16242,#16243,#16244,
#16245,#16246,#16247,#16248,#16249),.UNSPECIFIED.,.F.,.F.,(4,3,3,4),(-4.09202352044854,
-3.95441594380723,-2.96581195785542,-2.07317267331972),.UNSPECIFIED.);
#313=B_SPLINE_CURVE_WITH_KNOTS('',3,(#16252,#16253,#16254,#16255,#16256,
#16257,#16258),.UNSPECIFIED.,.F.,.F.,(4,3,4),(0.,0.98860398595181,1.12274180646091),
 .UNSPECIFIED.);
#314=B_SPLINE_CURVE_WITH_KNOTS('',3,(#16263,#16264,#16265,#16266,#16267,
#16268,#16269,#16270,#16271,#16272,#16273,#16274,#16275,#16276,#16277,#16278,
#16279,#16280,#16281,#16282,#16283,#16284),.UNSPECIFIED.,.F.,.F.,(4,3,3,
3,3,3,3,4),(-10.3752088276281,-9.88603985951807,-8.89743587356626,-7.90883188761445,
-6.92022790166265,-5.93162391571084,-4.94301992975903,-4.09202352044854),
 .UNSPECIFIED.);
#315=B_SPLINE_CURVE_WITH_KNOTS('',3,(#16285,#16286,#16287,#16288,#16289,
#16290,#16291,#16292,#16293,#16294,#16295,#16296,#16297,#16298,#16299,#16300,
#16301,#16302,#16303,#16304,#16305,#16306),.UNSPECIFIED.,.F.,.F.,(4,3,3,
3,3,3,3,4),(1.12274180646091,1.97720797190362,2.96581195785542,3.95441594380723,
4.94301992975904,5.93162391571084,6.92022790166265,7.4059271136405),
 .UNSPECIFIED.);
#316=B_SPLINE_CURVE_WITH_KNOTS('',3,(#16311,#16312,#16313,#16314,#16315,
#16316,#16317,#16318,#16319,#16320,#16321,#16322,#16323,#16324,#16325,#16326,
#16327,#16328,#16329,#16330,#16331,#16332),.UNSPECIFIED.,.F.,.F.,(4,3,3,
3,3,3,3,4),(-16.6583941348077,-15.8176637752289,-14.8290597892771,-13.8404558033253,
-12.8518518173735,-11.8632478314217,-10.8746438454699,-10.3752088276281),
 .UNSPECIFIED.);
#317=B_SPLINE_CURVE_WITH_KNOTS('',3,(#16333,#16334,#16335,#16336,#16337,
#16338,#16339,#16340,#16341,#16342,#16343,#16344,#16345,#16346,#16347,#16348,
#16349,#16350,#16351,#16352,#16353,#16354),.UNSPECIFIED.,.F.,.F.,(4,3,3,
3,3,3,3,4),(7.4059271136405,7.90883188761445,8.89743587356626,9.88603985951806,
10.8746438454699,11.8632478314217,12.8518518173735,13.6891124208201),
 .UNSPECIFIED.);
#318=B_SPLINE_CURVE_WITH_KNOTS('',3,(#16359,#16360,#16361,#16362,#16363,
#16364,#16365,#16366,#16367,#16368,#16369,#16370,#16371,#16372,#16373,#16374,
#16375,#16376,#16377,#16378,#16379,#16380,#16381,#16382,#16383),
 .UNSPECIFIED.,.F.,.F.,(4,3,3,3,3,3,3,3,4),(-22.9415794419873,-22.7378916768916,
-21.7492876909397,-20.7606837049879,-19.7720797190361,-18.7834757330843,
-17.7948717471325,-16.8062677611807,-16.6583941348077),.UNSPECIFIED.);
#319=B_SPLINE_CURVE_WITH_KNOTS('',3,(#16384,#16385,#16386,#16387,#16388,
#16389,#16390,#16391,#16392,#16393,#16394,#16395,#16396,#16397,#16398,#16399,
#16400,#16401,#16402,#16403,#16404,#16405,#16406,#16407,#16408),
 .UNSPECIFIED.,.F.,.F.,(4,3,3,3,3,3,3,3,4),(13.6891124208201,13.8404558033253,
14.8290597892771,15.8176637752289,16.8062677611807,17.7948717471325,18.7834757330843,
19.7720797190361,19.9722977279997),.UNSPECIFIED.);
#320=B_SPLINE_CURVE_WITH_KNOTS('',3,(#16413,#16414,#16415,#16416,#16417,
#16418,#16419,#16420,#16421,#16422,#16423,#16424,#16425,#16426,#16427,#16428,
#16429,#16430,#16431,#16432,#16433,#16434),.UNSPECIFIED.,.F.,.F.,(4,3,3,
3,3,3,3,4),(-29.2247647491669,-28.6695155926024,-27.6809116066506,-26.6923076206988,
-25.703703634747,-24.7150996487952,-23.7264956628434,-22.9415794419873),
 .UNSPECIFIED.);
#321=B_SPLINE_CURVE_WITH_KNOTS('',3,(#16435,#16436,#16437,#16438,#16439,
#16440,#16441,#16442,#16443,#16444,#16445,#16446,#16447,#16448,#16449,#16450,
#16451,#16452,#16453,#16454,#16455,#16456),.UNSPECIFIED.,.F.,.F.,(4,3,3,
3,3,3,3,4),(19.9722977279997,20.7606837049879,21.7492876909397,22.7378916768916,
23.7264956628434,24.7150996487952,25.703703634747,26.2554830351793),
 .UNSPECIFIED.);
#322=B_SPLINE_CURVE_WITH_KNOTS('',3,(#16461,#16462,#16463,#16464,#16465,
#16466,#16467,#16468,#16469,#16470,#16471,#16472,#16473,#16474,#16475,#16476,
#16477,#16478,#16479,#16480,#16481,#16482),.UNSPECIFIED.,.F.,.F.,(4,3,3,
3,3,3,3,4),(-35.5079500563465,-34.6011395083132,-33.6125355223614,-32.6239315364096,
-31.6353275504578,-30.646723564506,-29.6581195785542,-29.2247647491669),
 .UNSPECIFIED.);
#323=B_SPLINE_CURVE_WITH_KNOTS('',3,(#16483,#16484,#16485,#16486,#16487,
#16488,#16489,#16490,#16491,#16492,#16493,#16494,#16495,#16496,#16497,#16498,
#16499,#16500,#16501,#16502,#16503,#16504),.UNSPECIFIED.,.F.,.F.,(4,3,3,
3,3,3,3,4),(26.2554830351793,26.6923076206988,27.6809116066506,28.6695155926024,
29.6581195785542,30.646723564506,31.6353275504578,32.5386683423588),
 .UNSPECIFIED.);
#324=B_SPLINE_CURVE_WITH_KNOTS('',3,(#16509,#16510,#16511,#16512,#16513,
#16514,#16515,#16516,#16517,#16518,#16519,#16520,#16521,#16522,#16523,#16524,
#16525,#16526,#16527,#16528,#16529,#16530,#16531,#16532,#16533),
 .UNSPECIFIED.,.F.,.F.,(4,3,3,3,3,3,3,3,4),(-41.7911353635261,-41.5213674099759,
-40.5327634240241,-39.5441594380723,-38.5555554521205,-37.5669514661687,
-36.5783474802168,-35.589743494265,-35.5079500563465),.UNSPECIFIED.);
#325=B_SPLINE_CURVE_WITH_KNOTS('',3,(#16534,#16535,#16536,#16537,#16538,
#16539,#16540,#16541,#16542,#16543,#16544,#16545,#16546,#16547,#16548,#16549,
#16550,#16551,#16552,#16553,#16554,#16555,#16556,#16557,#16558),
 .UNSPECIFIED.,.F.,.F.,(4,3,3,3,3,3,3,3,4),(32.5386683423588,32.6239315364096,
33.6125355223614,34.6011395083132,35.589743494265,36.5783474802168,37.5669514661686,
38.5555554521205,38.8218536495384),.UNSPECIFIED.);
#326=B_SPLINE_CURVE_WITH_KNOTS('',3,(#16563,#16564,#16565,#16566,#16567,
#16568,#16569,#16570,#16571,#16572,#16573,#16574,#16575,#16576,#16577,#16578,
#16579,#16580,#16581,#16582,#16583,#16584),.UNSPECIFIED.,.F.,.F.,(4,3,3,
3,3,3,3,4),(-48.0743206707057,-47.4529913256867,-46.4643873397349,-45.4757833537831,
-44.4871793678313,-43.4985753818795,-42.5099713959277,-41.7911353635261),
 .UNSPECIFIED.);
#327=B_SPLINE_CURVE_WITH_KNOTS('',3,(#16585,#16586,#16587,#16588,#16589,
#16590,#16591,#16592,#16593,#16594,#16595,#16596,#16597,#16598,#16599,#16600,
#16601,#16602,#16603,#16604,#16605,#16606),.UNSPECIFIED.,.F.,.F.,(4,3,3,
3,3,3,3,4),(38.8218536495384,39.5441594380723,40.5327634240241,41.5213674099759,
42.5099713959277,43.4985753818795,44.4871793678313,45.105038956718),
 .UNSPECIFIED.);
#328=B_SPLINE_CURVE_WITH_KNOTS('',3,(#16611,#16612,#16613,#16614,#16615,
#16616,#16617,#16618,#16619,#16620,#16621,#16622,#16623,#16624,#16625,#16626,
#16627,#16628,#16629,#16630,#16631,#16632),.UNSPECIFIED.,.F.,.F.,(4,3,3,
3,3,3,3,4),(-54.3575059778853,-53.3846152413976,-52.3960112554458,-51.4074072694939,
-50.4188032835421,-49.4301992975903,-48.4415953116385,-48.0743206707057),
 .UNSPECIFIED.);
#329=B_SPLINE_CURVE_WITH_KNOTS('',3,(#16633,#16634,#16635,#16636,#16637,
#16638,#16639,#16640,#16641,#16642,#16643,#16644,#16645,#16646,#16647,#16648,
#16649,#16650,#16651,#16652,#16653,#16654),.UNSPECIFIED.,.F.,.F.,(4,3,3,
3,3,3,3,4),(45.105038956718,45.4757833537831,46.4643873397349,47.4529913256867,
48.4415953116385,49.4301992975903,50.4188032835421,51.3882242638976),
 .UNSPECIFIED.);
#330=B_SPLINE_CURVE_WITH_KNOTS('',3,(#16659,#16660,#16661,#16662,#16663,
#16664,#16665,#16666,#16667,#16668,#16669,#16670,#16671,#16672,#16673,#16674,
#16675,#16676,#16677,#16678,#16679,#16680,#16681,#16682,#16683),
 .UNSPECIFIED.,.F.,.F.,(4,3,3,3,3,3,3,3,4),(-60.6406912850648,-60.3048431430602,
-59.3162391571084,-58.3276351711566,-57.3390311852048,-56.350427199253,
-55.3618232133012,-54.3732192273494,-54.3575059778853),.UNSPECIFIED.);
#331=B_SPLINE_CURVE_WITH_KNOTS('',3,(#16684,#16685,#16686,#16687,#16688,
#16689,#16690,#16691,#16692,#16693,#16694,#16695,#16696,#16697,#16698,#16699,
#16700,#16701,#16702,#16703,#16704,#16705,#16706,#16707,#16708),
 .UNSPECIFIED.,.F.,.F.,(4,3,3,3,3,3,3,3,4),(51.3882242638976,51.4074072694939,
52.3960112554457,53.3846152413976,54.3732192273494,55.3618232133012,56.350427199253,
57.3390311852048,57.6714095710772),.UNSPECIFIED.);
#332=B_SPLINE_CURVE_WITH_KNOTS('',3,(#16713,#16714,#16715,#16716,#16717,
#16718,#16719,#16720,#16721,#16722,#16723,#16724,#16725,#16726,#16727,#16728,
#16729,#16730,#16731,#16732,#16733,#16734),.UNSPECIFIED.,.F.,.F.,(4,3,3,
3,3,3,3,4),(-66.9238765922444,-66.236467058771,-65.2478630728192,-64.2592590868674,
-63.2706551009156,-62.2820511149638,-61.293447129012,-60.6406912850648),
 .UNSPECIFIED.);
#333=B_SPLINE_CURVE_WITH_KNOTS('',3,(#16735,#16736,#16737,#16738,#16739,
#16740,#16741,#16742,#16743,#16744,#16745,#16746,#16747,#16748,#16749,#16750,
#16751,#16752,#16753,#16754,#16755,#16756),.UNSPECIFIED.,.F.,.F.,(4,3,3,
3,3,3,3,4),(57.6714095710772,58.3276351711566,59.3162391571084,60.3048431430602,
61.293447129012,62.2820511149638,63.2706551009156,63.9545948782568),
 .UNSPECIFIED.);
#334=B_SPLINE_CURVE_WITH_KNOTS('',3,(#16761,#16762,#16763,#16764,#16765,
#16766,#16767,#16768,#16769,#16770,#16771,#16772,#16773,#16774,#16775,#16776,
#16777,#16778,#16779,#16780,#16781,#16782,#16783,#16784,#16785),
 .UNSPECIFIED.,.F.,.F.,(4,3,3,3,3,3,3,3,4),(-73.207061899424,-73.1566949604337,
-72.1680909744819,-71.1794869885301,-70.1908830025783,-69.2022790166264,
-68.2136750306747,-67.2250710447229,-66.9238765922444),.UNSPECIFIED.);
#335=B_SPLINE_CURVE_WITH_KNOTS('',3,(#16786,#16787,#16788,#16789,#16790,
#16791,#16792,#16793,#16794,#16795,#16796,#16797,#16798,#16799,#16800,#16801,
#16802,#16803,#16804,#16805,#16806,#16807,#16808,#16809,#16810),
 .UNSPECIFIED.,.F.,.F.,(4,3,3,3,3,3,3,3,4),(63.9545948782568,64.2592590868674,
65.2478630728192,66.236467058771,67.2250710447228,68.2136750306746,69.2022790166264,
70.1908830025782,70.2377801854364),.UNSPECIFIED.);
#336=B_SPLINE_CURVE_WITH_KNOTS('',3,(#16816,#16817,#16818,#16819,#16820,
#16821),.UNSPECIFIED.,.F.,.F.,(4,1,1,4),(84.8230016469244,85.7612386938859,
86.7498426798377,87.6424819643734),.UNSPECIFIED.);
#337=B_SPLINE_CURVE_WITH_KNOTS('',3,(#16824,#16825,#16826,#16827,#16828),
 .UNSPECIFIED.,.F.,.F.,(4,1,4),(84.8230016469244,85.4131470585492,86.401751044501),
 .UNSPECIFIED.);
#338=B_SPLINE_CURVE_WITH_KNOTS('',3,(#16833,#16834,#16835,#16836,#16837,
#16838,#16839,#16840,#16841,#16842,#16843),.UNSPECIFIED.,.F.,.F.,(4,1,1,
1,1,1,1,1,4),(78.5398163397448,78.8410107922232,79.829614778175,80.8182187641268,
81.8068227500786,82.7954267360304,83.7840307219822,84.7726347079341,84.8230016469244),
 .UNSPECIFIED.);
#339=B_SPLINE_CURVE_WITH_KNOTS('',3,(#16844,#16845,#16846,#16847,#16848,
#16849,#16850,#16851,#16852,#16853),.UNSPECIFIED.,.F.,.F.,(4,1,1,1,1,1,
1,4),(78.5398163397448,79.4815231428384,80.4701271287902,81.458731114742,
82.4473351006938,83.4359390866456,84.4245430725974,84.8230016469244),
 .UNSPECIFIED.);
#340=B_SPLINE_CURVE_WITH_KNOTS('',3,(#16858,#16859,#16860,#16861,#16862,
#16863,#16864,#16865,#16866,#16867),.UNSPECIFIED.,.F.,.F.,(4,1,1,1,1,1,
1,4),(72.2566310325652,72.9093868765124,73.8979908624642,74.886594848416,
75.8751988343678,76.8638028203196,77.8524068062714,78.5398163397448),
 .UNSPECIFIED.);
#341=B_SPLINE_CURVE_WITH_KNOTS('',3,(#16868,#16869,#16870,#16871,#16872,
#16873,#16874,#16875,#16876,#16877,#16878),.UNSPECIFIED.,.F.,.F.,(4,1,1,
1,1,1,1,1,4),(72.2566310325652,72.5612952411758,73.5498992271276,74.5385032130794,
75.5271071990312,76.515711184983,77.5043151709348,78.4929191568866,78.5398163397448),
 .UNSPECIFIED.);
#342=B_SPLINE_CURVE_WITH_KNOTS('',3,(#16883,#16884,#16885,#16886,#16887,
#16888,#16889,#16890,#16891,#16892,#16893),.UNSPECIFIED.,.F.,.F.,(4,1,1,
1,1,1,1,1,4),(65.9734457253856,65.9891589748497,66.9777629608015,67.9663669467533,
68.9549709327052,69.943574918657,70.9321789046088,71.9207828905606,72.2566310325652),
 .UNSPECIFIED.);
#343=B_SPLINE_CURVE_WITH_KNOTS('',3,(#16894,#16895,#16896,#16897,#16898,
#16899,#16900,#16901,#16902,#16903),.UNSPECIFIED.,.F.,.F.,(4,1,1,1,1,1,
1,4),(65.9734457253856,66.6296713254649,67.6182753114167,68.6068792973685,
69.5954832833203,70.5840872692721,71.5726912552239,72.2566310325652),
 .UNSPECIFIED.);
#344=B_SPLINE_CURVE_WITH_KNOTS('',3,(#16908,#16909,#16910,#16911,#16912,
#16913,#16914,#16915,#16916,#16917),.UNSPECIFIED.,.F.,.F.,(4,1,1,1,1,1,
1,4),(59.6902604182061,60.0575350591389,61.0461390450907,62.0347430310425,
63.0233470169943,64.0119510029461,65.0005549888979,65.9734457253856),
 .UNSPECIFIED.);
#345=B_SPLINE_CURVE_WITH_KNOTS('',3,(#16918,#16919,#16920,#16921,#16922,
#16923,#16924,#16925,#16926,#16927,#16928),.UNSPECIFIED.,.F.,.F.,(4,1,1,
1,1,1,1,1,4),(59.690260418206,59.7094434238023,60.6980474097541,61.6866513957059,
62.6752553816577,63.6638593676095,64.6524633535613,65.6410673395131,65.9734457253856),
 .UNSPECIFIED.);
#346=B_SPLINE_CURVE_WITH_KNOTS('',3,(#16933,#16934,#16935,#16936,#16937,
#16938,#16939,#16940,#16941,#16942),.UNSPECIFIED.,.F.,.F.,(4,1,1,1,1,1,
1,4),(53.4070751110265,54.1259111434281,55.1145151293799,56.1031191153317,
57.0917231012835,58.0803270872353,59.0689310731871,59.6902604182061),
 .UNSPECIFIED.);
#347=B_SPLINE_CURVE_WITH_KNOTS('',3,(#16943,#16944,#16945,#16946,#16947,
#16948,#16949,#16950,#16951,#16952),.UNSPECIFIED.,.F.,.F.,(4,1,1,1,1,1,
1,4),(53.4070751110264,53.7778195080914,54.7664234940432,55.755027479995,
56.7436314659468,57.7322354518986,58.7208394378505,59.690260418206),
 .UNSPECIFIED.);
#348=B_SPLINE_CURVE_WITH_KNOTS('',3,(#16957,#16958,#16959,#16960,#16961,
#16962,#16963,#16964,#16965,#16966,#16967),.UNSPECIFIED.,.F.,.F.,(4,1,1,
1,1,1,1,1,4),(47.1238898038469,47.2056832417654,48.1942872277172,49.182891213669,
50.1714951996208,51.1600991855726,52.1487031715244,53.1373071574762,53.4070751110265),
 .UNSPECIFIED.);
#349=B_SPLINE_CURVE_WITH_KNOTS('',3,(#16968,#16969,#16970,#16971,#16972,
#16973,#16974,#16975,#16976,#16977),.UNSPECIFIED.,.F.,.F.,(4,1,1,1,1,1,
1,4),(47.1238898038468,47.8461955923806,48.8347995783324,49.8234035642842,
50.812007550236,51.8006115361878,52.7892155221396,53.4070751110264),
 .UNSPECIFIED.);
#350=B_SPLINE_CURVE_WITH_KNOTS('',3,(#16982,#16983,#16984,#16985,#16986,
#16987,#16988,#16989,#16990,#16991),.UNSPECIFIED.,.F.,.F.,(4,1,1,1,1,1,
1,4),(40.8407044966673,41.2740593260546,42.2626633120064,43.2512672979582,
44.23987128391,45.2284752698618,46.2170792558136,47.1238898038469),
 .UNSPECIFIED.);
#351=B_SPLINE_CURVE_WITH_KNOTS('',3,(#16992,#16993,#16994,#16995,#16996,
#16997,#16998,#16999,#17000,#17001,#17002),.UNSPECIFIED.,.F.,.F.,(4,1,1,
1,1,1,1,1,4),(40.8407044966673,40.9259676907179,41.9145716766698,42.9031756626216,
43.8917796485734,44.8803836345252,45.868987620477,46.8575916064288,47.1238898038468),
 .UNSPECIFIED.);
#352=B_SPLINE_CURVE_WITH_KNOTS('',3,(#17007,#17008,#17009,#17010,#17011,
#17012,#17013,#17014,#17015,#17016),.UNSPECIFIED.,.F.,.F.,(4,1,1,1,1,1,
1,4),(34.5575191894877,35.3424354103437,36.3310393962955,37.3196433822473,
38.3082473681991,39.296851354151,40.2854553401028,40.8407044966673),
 .UNSPECIFIED.);
#353=B_SPLINE_CURVE_WITH_KNOTS('',3,(#17017,#17018,#17019,#17020,#17021,
#17022,#17023,#17024,#17025,#17026),.UNSPECIFIED.,.F.,.F.,(4,1,1,1,1,1,
1,4),(34.5575191894877,34.9943437750071,35.9829477609589,36.9715517469107,
37.9601557328625,38.9487597188143,39.9373637047661,40.8407044966673),
 .UNSPECIFIED.);
#354=B_SPLINE_CURVE_WITH_KNOTS('',3,(#17031,#17032,#17033,#17034,#17035,
#17036,#17037,#17038,#17039,#17040,#17041),.UNSPECIFIED.,.F.,.F.,(4,1,1,
1,1,1,1,1,4),(28.2743338823081,28.4222075086811,29.4108114946329,30.3994154805847,
31.3880194665365,32.3766234524883,33.3652274384401,34.3538314243919,34.5575191894877),
 .UNSPECIFIED.);
#355=B_SPLINE_CURVE_WITH_KNOTS('',3,(#17042,#17043,#17044,#17045,#17046,
#17047,#17048,#17049,#17050,#17051),.UNSPECIFIED.,.F.,.F.,(4,1,1,1,1,1,
1,4),(28.2743338823081,29.0627198592963,30.0513238452481,31.0399278311999,
32.0285318171517,33.0171358031035,34.0057397890553,34.5575191894877),
 .UNSPECIFIED.);
#356=B_SPLINE_CURVE_WITH_KNOTS('',3,(#17056,#17057,#17058,#17059,#17060,
#17061,#17062,#17063,#17064,#17065),.UNSPECIFIED.,.F.,.F.,(4,1,1,1,1,1,
1,4),(21.9911485751285,22.4905835929702,23.479187578922,24.4677915648739,
25.4563955508257,26.4449995367775,27.4336035227293,28.2743338823081),
 .UNSPECIFIED.);
#357=B_SPLINE_CURVE_WITH_KNOTS('',3,(#17066,#17067,#17068,#17069,#17070,
#17071,#17072,#17073,#17074,#17075,#17076),.UNSPECIFIED.,.F.,.F.,(4,1,1,
1,1,1,1,1,4),(21.9911485751285,22.1424919576336,23.1310959435854,24.1196999295372,
25.108303915489,26.0969079014409,27.0855118873927,28.0741158733445,28.2743338823081),
 .UNSPECIFIED.);
#358=B_SPLINE_CURVE_WITH_KNOTS('',3,(#17081,#17082,#17083,#17084,#17085,
#17086,#17087,#17088,#17089,#17090),.UNSPECIFIED.,.F.,.F.,(4,1,1,1,1,1,
1,4),(15.7079632679489,16.5589596772594,17.5475636632112,18.536167649163,
19.5247716351148,20.5133756210666,21.5019796070184,21.9911485751285),
 .UNSPECIFIED.);
#359=B_SPLINE_CURVE_WITH_KNOTS('',3,(#17091,#17092,#17093,#17094,#17095,
#17096,#17097,#17098,#17099,#17100),.UNSPECIFIED.,.F.,.F.,(4,1,1,1,1,1,
1,4),(15.7079632679489,16.2108680419228,17.1994720278746,18.1880760138264,
19.1766799997782,20.16528398573,21.1538879716818,21.9911485751285),
 .UNSPECIFIED.);
#360=B_SPLINE_CURVE_WITH_KNOTS('',3,(#17103,#17104,#17105,#17106,#17107,
#17108,#17109,#17110,#17111,#17112,#17113,#17114,#17115,#17116,#17117,#17118,
#17119,#17120,#17121,#17122,#17123,#17124,#17125,#17126,#17127,#17128,#17129,
#17130,#17131,#17132,#17133,#17134,#17135,#17136,#17137,#17138,#17139,#17140,
#17141,#17142,#17143,#17144,#17145,#17146,#17147,#17148,#17149,#17150,#17151,
#17152,#17153,#17154,#17155,#17156,#17157,#17158,#17159,#17160,#17161,#17162,
#17163,#17164,#17165,#17166,#17167,#17168,#17169,#17170,#17171,#17172,#17173,
#17174,#17175,#17176,#17177,#17178,#17179,#17180,#17181,#17182,#17183,#17184,
#17185,#17186,#17187),.UNSPECIFIED.,.F.,.F.,(4,3,3,3,3,3,3,3,3,3,3,3,3,
3,3,3,3,3,3,3,3,3,3,3,3,3,3,3,4),(-0.27663179171271,-0.2651301030347,-0.250460786414225,
-0.245045718144737,-0.241800530081285,-0.226536328657412,-0.215620637943102,
-0.212140369574972,-0.209334257433326,-0.193597942693264,-0.177548592082217,
-0.167964144797397,-0.163147554742663,-0.159540919290815,-0.14301553793474,
-0.139210802942938,-0.123238048148458,-0.115535670139179,-0.110632353224551,
-0.107705074830832,-0.0911577161793469,-0.074249565407069,-0.064760271735975,
-0.0583780708391448,-0.053731028480074,-0.0362740667018561,-0.018137033350928,
-0.00108826469303175,0.),.UNSPECIFIED.);
#361=B_SPLINE_CURVE_WITH_KNOTS('',3,(#17192,#17193,#17194,#17195,#17196,
#17197,#17198,#17199,#17200,#17201,#17202,#17203,#17204,#17205,#17206,#17207,
#17208,#17209,#17210,#17211,#17212,#17213,#17214,#17215,#17216,#17217,#17218,
#17219,#17220,#17221,#17222,#17223,#17224,#17225,#17226,#17227,#17228,#17229,
#17230,#17231,#17232,#17233,#17234,#17235,#17236,#17237,#17238,#17239,#17240,
#17241,#17242,#17243,#17244,#17245,#17246,#17247,#17248,#17249,#17250,#17251,
#17252,#17253,#17254,#17255,#17256,#17257,#17258,#17259,#17260,#17261,#17262,
#17263,#17264,#17265,#17266,#17267,#17268,#17269,#17270,#17271,#17272,#17273),
 .UNSPECIFIED.,.F.,.F.,(4,3,3,3,3,3,3,3,3,3,3,3,3,3,3,3,3,3,3,3,3,3,3,3,
3,3,3,4),(-0.275362278356885,-0.261358215039034,-0.24420947844022,-0.239226268528359,
-0.234169052699615,-0.216973772971366,-0.205373091631011,-0.200128212738553,
-0.196878691185682,-0.180126653267857,-0.163783011764808,-0.153879339385736,
-0.149003330340905,-0.145912671051637,-0.130035116133936,-0.124168322248522,
-0.108234162937227,-0.100893521573436,-0.0956516943326387,-0.0926034073274861,
-0.0768394523952997,-0.0611489821427944,-0.0532954156811162,-0.0475078582072449,
-0.0447093270180608,-0.0295993550201047,-0.0147996775100523,0.),
 .UNSPECIFIED.);
#362=B_SPLINE_CURVE_WITH_KNOTS('',3,(#17602,#17603,#17604,#17605,#17606,
#17607,#17608,#17609,#17610,#17611,#17612,#17613,#17614,#17615,#17616,#17617,
#17618,#17619,#17620),.UNSPECIFIED.,.F.,.F.,(4,3,3,3,3,3,4),(70.2377801854364,
71.1794869885301,72.1680909744818,73.1566949604337,74.1452989463855,75.1339029323373,
76.026542216873),.UNSPECIFIED.);
#363=B_SPLINE_CURVE_WITH_KNOTS('',3,(#17622,#17623,#17624,#17625,#17626,
#17627,#17628,#17629,#17630,#17631,#17632,#17633,#17634,#17635,#17636,#17637,
#17638,#17639,#17640,#17641,#17642,#17643,#17644,#17645,#17646,#17647,#17648,
#17649,#17650,#17651,#17652,#17653,#17654,#17655,#17656,#17657,#17658,#17659,
#17660,#17661,#17662,#17663,#17664,#17665,#17666,#17667,#17668,#17669,#17670,
#17671,#17672,#17673,#17674,#17675,#17676,#17677,#17678,#17679,#17680,#17681,
#17682,#17683,#17684,#17685,#17686,#17687,#17688,#17689,#17690,#17691,#17692,
#17693,#17694,#17695,#17696,#17697,#17698,#17699,#17700,#17701,#17702,#17703,
#17704,#17705,#17706),.UNSPECIFIED.,.F.,.F.,(4,3,3,3,3,3,3,3,3,3,3,3,3,
3,3,3,3,3,3,3,3,3,3,3,3,3,3,3,4),(-0.276631791712721,-0.265130103034713,
-0.250460792531934,-0.24504572637101,-0.241800547465848,-0.226536350695918,
-0.215620657226796,-0.212140587651992,-0.209334513885687,-0.193598209427458,
-0.177548857689101,-0.167964344002561,-0.163147689853096,-0.159540965946658,
-0.143015584324094,-0.139210802942942,-0.123238050693282,-0.115535672524952,
-0.110632355020678,-0.107705075837133,-0.0911577201523597,-0.0742495721522352,
-0.064760273687438,-0.0583780759534126,-0.0537310263259031,-0.0362740663814007,
-0.0181370331907004,-0.00108825577301921,0.),.UNSPECIFIED.);
#364=B_SPLINE_CURVE_WITH_KNOTS('',3,(#17707,#17708,#17709,#17710,#17711,
#17712,#17713,#17714,#17715),.UNSPECIFIED.,.F.,.F.,(4,1,1,1,1,1,4),(10.375208827628,
11.2678481121638,12.2564520981156,13.2450560840674,14.2336600700192,15.222264055971,
15.7079632679489),.UNSPECIFIED.);
#365=B_SPLINE_CURVE_WITH_KNOTS('',3,(#17721,#17722,#17723,#17724,#17725,
#17726,#17727,#17728,#17729,#17730,#17731,#17732,#17733,#17734,#17735,#17736,
#17737,#17738,#17739,#17740,#17741,#17742,#17743,#17744,#17745,#17746,#17747,
#17748,#17749,#17750,#17751,#17752,#17753,#17754,#17755,#17756,#17757,#17758,
#17759,#17760,#17761,#17762,#17763,#17764,#17765,#17766,#17767,#17768,#17769,
#17770,#17771,#17772,#17773,#17774,#17775,#17776,#17777,#17778,#17779,#17780,
#17781,#17782,#17783,#17784,#17785,#17786,#17787,#17788,#17789,#17790,#17791,
#17792,#17793,#17794,#17795,#17796,#17797,#17798,#17799,#17800,#17801,#17802),
 .UNSPECIFIED.,.F.,.F.,(4,3,3,3,3,3,3,3,3,3,3,3,3,3,3,3,3,3,3,3,3,3,3,3,
3,3,3,4),(-0.275362278356884,-0.26135821503903,-0.244209478440216,-0.239226264711111,
-0.234169052469442,-0.216973772681103,-0.20537309137703,-0.200128210040024,
-0.196878689389314,-0.180126650893078,-0.163783003806357,-0.153879333416897,
-0.149003310760071,-0.145912654690853,-0.130035094652386,-0.124168322248516,
-0.108234162817484,-0.100893518944725,-0.0956516935782954,-0.0926034075571851,
-0.0768394511997701,-0.061148985158665,-0.0532954165631934,-0.0475078611084516,
-0.0447093297178545,-0.0295993633295068,-0.0147996816647534,0.),
 .UNSPECIFIED.);
#366=B_SPLINE_CURVE_WITH_KNOTS('',3,(#17805,#17806,#17807,#17808,#17809,
#17810,#17811,#17812),.UNSPECIFIED.,.F.,.F.,(4,1,1,1,1,4),(11.6159397475004,
12.6045437334522,13.593147719404,14.5817517053558,15.5703556913076,15.7079632679489),
 .UNSPECIFIED.);
#367=B_SPLINE_CURVE_WITH_KNOTS('',3,(#18141,#18142,#18143,#18144,#18145,
#18146,#18147,#18148,#18149,#18150,#18151,#18152,#18153,#18154,#18155,#18156),
 .UNSPECIFIED.,.F.,.F.,(4,3,3,3,3,4),(-78.0997148901927,-77.1111109042409,
-76.1225069182891,-75.1339029323373,-74.1452989463855,-73.207061899424),
 .UNSPECIFIED.);
#368=CONICAL_SURFACE('',#9304,3.9,0.785398163397444);
#369=CONICAL_SURFACE('',#9308,3.9,0.785398163397444);
#370=CONICAL_SURFACE('',#9312,3.9,0.78539816339745);
#371=CONICAL_SURFACE('',#9316,3.9,0.78539816339745);
#372=CONICAL_SURFACE('',#9332,3.92928932188135,0.392699081698714);
#373=CONICAL_SURFACE('',#9335,3.92928932188135,0.392699081698714);
#374=CONICAL_SURFACE('',#9338,3.92928932188135,0.392699081698713);
#375=CONICAL_SURFACE('',#9342,3.92928932188135,0.392699081698724);
#376=CONICAL_SURFACE('',#9346,3.75,0.785398163397449);
#377=CONICAL_SURFACE('',#9349,3.75,0.785398163397447);
#378=CONICAL_SURFACE('',#9354,3.27928932188134,1.17809724509616);
#379=CONICAL_SURFACE('',#9358,3.47071067811865,1.17809724509617);
#380=CONICAL_SURFACE('',#9361,2.475,0.785398163397448);
#381=CONICAL_SURFACE('',#9363,3.27928932188134,1.17809724509616);
#382=CONICAL_SURFACE('',#9367,3.47071067811866,1.17809724509617);
#383=CONICAL_SURFACE('',#9369,2.475,0.785398163397448);
#384=CONICAL_SURFACE('',#9371,3.27928932188134,1.17809724509614);
#385=CONICAL_SURFACE('',#9378,2.475,0.785398163397449);
#386=CONICAL_SURFACE('',#9380,3.27928932188134,1.17809724509614);
#387=CONICAL_SURFACE('',#9382,2.475,0.785398163397449);
#388=CONICAL_SURFACE('',#9388,3.47071067811866,1.17809724509616);
#389=CONICAL_SURFACE('',#9390,3.47071067811866,1.17809724509616);
#390=CONICAL_SURFACE('',#9393,3.75,0.785398163397449);
#391=CONICAL_SURFACE('',#9395,3.75,0.785398163397449);
#392=CONICAL_SURFACE('',#9472,3.9,0.78539816339746);
#393=CONICAL_SURFACE('',#9476,3.9,0.785398163397461);
#394=CONICAL_SURFACE('',#9480,3.9,0.785398163397455);
#395=CONICAL_SURFACE('',#9484,3.9,0.785398163397455);
#396=CONICAL_SURFACE('',#9499,3.27928932188134,1.17809724509612);
#397=CONICAL_SURFACE('',#9511,2.475,0.785398163397451);
#398=CONICAL_SURFACE('',#9514,3.9,0.785398163397461);
#399=CONICAL_SURFACE('',#9517,3.9,0.785398163397455);
#400=CONICAL_SURFACE('',#9519,3.9,0.785398163397455);
#401=CONICAL_SURFACE('',#9521,3.9,0.78539816339746);
#402=CONICAL_SURFACE('',#9526,3.27928932188135,1.17809724509617);
#403=CONICAL_SURFACE('',#9528,2.475,0.78539816339745);
#404=CONICAL_SURFACE('',#9530,3.27928932188135,1.17809724509617);
#405=CONICAL_SURFACE('',#9532,2.475,0.78539816339745);
#406=CONICAL_SURFACE('',#9534,3.27928932188134,1.17809724509612);
#407=CONICAL_SURFACE('',#9536,2.475,0.785398163397451);
#408=CONICAL_SURFACE('',#9545,1.8,0.785398163397447);
#409=CONICAL_SURFACE('',#9553,1.8,0.785398163397447);
#410=CONICAL_SURFACE('',#9564,1.8,0.785398163397439);
#411=CONICAL_SURFACE('',#9572,1.8,0.785398163397439);
#412=CONICAL_SURFACE('',#9667,13.65,0.785398163397449);
#413=CONICAL_SURFACE('',#9671,13.65,0.785398163397442);
#414=CONICAL_SURFACE('',#9675,13.65,0.785398163397449);
#415=CONICAL_SURFACE('',#9683,4.75,0.785398163397446);
#416=CONICAL_SURFACE('',#9695,13.65,0.78539816339745);
#417=CONICAL_SURFACE('',#9697,13.725,0.785398163397447);
#418=CONICAL_SURFACE('',#9704,13.65,0.78539816339745);
#419=CONICAL_SURFACE('',#9710,4.75,0.785398163397449);
#420=CONICAL_SURFACE('',#9714,8.35,0.785398163397449);
#421=CONICAL_SURFACE('',#9730,3.75,0.785398163397447);
#422=CONICAL_SURFACE('',#9738,3.75,0.785398163397447);
#423=CONICAL_SURFACE('',#9741,3.75,0.785398163397447);
#424=CONICAL_SURFACE('',#9748,3.75,0.785398163397447);
#425=CONICAL_SURFACE('',#9792,3.75,0.785398163397448);
#426=CONICAL_SURFACE('',#9816,3.75,0.785398163397447);
#427=CONICAL_SURFACE('',#9831,3.75,0.785398163397447);
#428=CONICAL_SURFACE('',#9834,3.75,0.785398163397448);
#429=CONICAL_SURFACE('',#9846,9.75,0.785398163397449);
#430=CONICAL_SURFACE('',#9878,1.75,0.785398163397449);
#431=CONICAL_SURFACE('',#9881,1.85,0.785398163397448);
#432=CONICAL_SURFACE('',#9919,0.5,1.02242932542481);
#433=CONICAL_SURFACE('',#9930,1.35,0.785398163397448);
#434=CONICAL_SURFACE('',#9933,2.325,0.785398163397448);
#435=CONICAL_SURFACE('',#9939,2.25,0.785398163397448);
#436=CONICAL_SURFACE('',#9943,2.25,0.78539816339745);
#437=SHAPE_REPRESENTATION_RELATIONSHIP('SRR','None',#18339,#450);
#438=SHAPE_REPRESENTATION_RELATIONSHIP('SRR','None',#18340,#451);
#439=SHAPE_REPRESENTATION_RELATIONSHIP('SRR','None',#18341,#452);
#440=SHAPE_REPRESENTATION_RELATIONSHIP('SRR','None',#18342,#453);
#441=SHAPE_REPRESENTATION_RELATIONSHIP('SRR','None',#18343,#454);
#442=SHAPE_REPRESENTATION_RELATIONSHIP('SRR','None',#18344,#455);
#443=SHAPE_REPRESENTATION_RELATIONSHIP('SRR','None',#18345,#456);
#444=SHAPE_REPRESENTATION_RELATIONSHIP('SRR','None',#18346,#457);
#445=SHAPE_REPRESENTATION_RELATIONSHIP('SRR','None',#18347,#458);
#446=SHAPE_REPRESENTATION_RELATIONSHIP('SRR','None',#18348,#459);
#447=SHAPE_REPRESENTATION_RELATIONSHIP('SRR','None',#18349,#460);
#448=SHAPE_REPRESENTATION_RELATIONSHIP('SRR','None',#18350,#461);
#449=SHAPE_REPRESENTATION_RELATIONSHIP('SRR','None',#18351,#462);
#450=ADVANCED_BREP_SHAPE_REPRESENTATION('',(#481),#18268);
#451=ADVANCED_BREP_SHAPE_REPRESENTATION('',(#482),#18269);
#452=ADVANCED_BREP_SHAPE_REPRESENTATION('',(#483),#18270);
#453=ADVANCED_BREP_SHAPE_REPRESENTATION('',(#484),#18271);
#454=ADVANCED_BREP_SHAPE_REPRESENTATION('',(#485),#18272);
#455=ADVANCED_BREP_SHAPE_REPRESENTATION('',(#486),#18273);
#456=ADVANCED_BREP_SHAPE_REPRESENTATION('',(#487),#18274);
#457=ADVANCED_BREP_SHAPE_REPRESENTATION('',(#488),#18275);
#458=ADVANCED_BREP_SHAPE_REPRESENTATION('',(#489),#18276);
#459=ADVANCED_BREP_SHAPE_REPRESENTATION('',(#490),#18277);
#460=ADVANCED_BREP_SHAPE_REPRESENTATION('',(#491),#18278);
#461=ADVANCED_BREP_SHAPE_REPRESENTATION('',(#492),#18279);
#462=ADVANCED_BREP_SHAPE_REPRESENTATION('',(#493),#18280);
#463=STYLED_ITEM('',(#18467),#481);
#464=STYLED_ITEM('',(#18467),#482);
#465=STYLED_ITEM('',(#18488),#483);
#466=STYLED_ITEM('',(#18467),#484);
#467=STYLED_ITEM('',(#18453),#8809);
#468=STYLED_ITEM('',(#18453),#8821);
#469=STYLED_ITEM('',(#18453),#8888);
#470=STYLED_ITEM('',(#18453),#8889);
#471=STYLED_ITEM('',(#18453),#8890);
#472=STYLED_ITEM('',(#18453),#485);
#473=STYLED_ITEM('',(#18460),#486);
#474=STYLED_ITEM('',(#18474),#487);
#475=STYLED_ITEM('',(#18488),#488);
#476=STYLED_ITEM('',(#18488),#489);
#477=STYLED_ITEM('',(#18488),#490);
#478=STYLED_ITEM('',(#18481),#491);
#479=STYLED_ITEM('',(#18481),#492);
#480=STYLED_ITEM('',(#18474),#493);
#481=MANIFOLD_SOLID_BREP('Body1',#9085);
#482=MANIFOLD_SOLID_BREP('Body1',#9086);
#483=MANIFOLD_SOLID_BREP('Body1',#9087);
#484=MANIFOLD_SOLID_BREP('Body1',#9088);
#485=MANIFOLD_SOLID_BREP('Body1',#9089);
#486=MANIFOLD_SOLID_BREP('Body1',#9090);
#487=MANIFOLD_SOLID_BREP('Body1',#9091);
#488=MANIFOLD_SOLID_BREP('Body1',#9092);
#489=MANIFOLD_SOLID_BREP('Body1',#9093);
#490=MANIFOLD_SOLID_BREP('Body1',#9094);
#491=MANIFOLD_SOLID_BREP('Body1',#9095);
#492=MANIFOLD_SOLID_BREP('Body1',#9096);
#493=MANIFOLD_SOLID_BREP('Body1',#9097);
#494=CYLINDRICAL_SURFACE('',#9267,2.5);
#495=CYLINDRICAL_SURFACE('',#9269,2.5);
#496=CYLINDRICAL_SURFACE('',#9271,2.5);
#497=CYLINDRICAL_SURFACE('',#9273,14.);
#498=CYLINDRICAL_SURFACE('',#9298,14.);
#499=CYLINDRICAL_SURFACE('',#9319,4.);
#500=CYLINDRICAL_SURFACE('',#9322,4.);
#501=CYLINDRICAL_SURFACE('',#9462,1.7);
#502=CYLINDRICAL_SURFACE('',#9463,1.7);
#503=CYLINDRICAL_SURFACE('',#9464,1.7);
#504=CYLINDRICAL_SURFACE('',#9465,1.7);
#505=CYLINDRICAL_SURFACE('',#9466,6.5);
#506=CYLINDRICAL_SURFACE('',#9467,4.);
#507=CYLINDRICAL_SURFACE('',#9468,4.);
#508=CYLINDRICAL_SURFACE('',#9487,4.);
#509=CYLINDRICAL_SURFACE('',#9490,4.);
#510=CYLINDRICAL_SURFACE('',#9524,4.);
#511=CYLINDRICAL_SURFACE('',#9538,1.7);
#512=CYLINDRICAL_SURFACE('',#9539,1.7);
#513=CYLINDRICAL_SURFACE('',#9540,1.7);
#514=CYLINDRICAL_SURFACE('',#9541,1.7);
#515=CYLINDRICAL_SURFACE('',#9542,6.5);
#516=CYLINDRICAL_SURFACE('',#9543,4.);
#517=CYLINDRICAL_SURFACE('',#9551,1.55);
#518=CYLINDRICAL_SURFACE('',#9555,1.55);
#519=CYLINDRICAL_SURFACE('',#9570,1.55);
#520=CYLINDRICAL_SURFACE('',#9574,1.55);
#521=CYLINDRICAL_SURFACE('',#9598,14.);
#522=CYLINDRICAL_SURFACE('',#9660,2.5);
#523=CYLINDRICAL_SURFACE('',#9661,2.5);
#524=CYLINDRICAL_SURFACE('',#9662,2.5);
#525=CYLINDRICAL_SURFACE('',#9669,13.9);
#526=CYLINDRICAL_SURFACE('',#9679,13.9);
#527=CYLINDRICAL_SURFACE('',#9691,5.);
#528=CYLINDRICAL_SURFACE('',#9702,13.9);
#529=CYLINDRICAL_SURFACE('',#9708,5.);
#530=CYLINDRICAL_SURFACE('',#9720,8.5);
#531=CYLINDRICAL_SURFACE('',#9722,5.025);
#532=CYLINDRICAL_SURFACE('',#9726,6.5);
#533=CYLINDRICAL_SURFACE('',#9752,2.05);
#534=CYLINDRICAL_SURFACE('',#9753,10.);
#535=CYLINDRICAL_SURFACE('',#9823,4.);
#536=CYLINDRICAL_SURFACE('',#9825,4.);
#537=CYLINDRICAL_SURFACE('',#9828,4.);
#538=CYLINDRICAL_SURFACE('',#9838,4.);
#539=CYLINDRICAL_SURFACE('',#9842,5.025);
#540=CYLINDRICAL_SURFACE('',#9848,1.954);
#541=CYLINDRICAL_SURFACE('',#9850,1.954);
#542=CYLINDRICAL_SURFACE('',#9851,1.954);
#543=CYLINDRICAL_SURFACE('',#9852,1.954);
#544=CYLINDRICAL_SURFACE('',#9853,1.954);
#545=CYLINDRICAL_SURFACE('',#9854,1.5555);
#546=CYLINDRICAL_SURFACE('',#9856,1.5555);
#547=CYLINDRICAL_SURFACE('',#9858,1.5555);
#548=CYLINDRICAL_SURFACE('',#9859,1.5555);
#549=CYLINDRICAL_SURFACE('',#9860,1.5555);
#550=CYLINDRICAL_SURFACE('',#9868,1.5555);
#551=CYLINDRICAL_SURFACE('',#9879,1.954);
#552=CYLINDRICAL_SURFACE('',#9885,1.4635);
#553=CYLINDRICAL_SURFACE('',#9887,1.4635);
#554=CYLINDRICAL_SURFACE('',#9888,1.4635);
#555=CYLINDRICAL_SURFACE('',#9889,1.4635);
#556=CYLINDRICAL_SURFACE('',#9890,1.4635);
#557=CYLINDRICAL_SURFACE('',#9891,1.4635);
#558=CYLINDRICAL_SURFACE('',#9892,1.4635);
#559=CYLINDRICAL_SURFACE('',#9893,1.4635);
#560=CYLINDRICAL_SURFACE('',#9894,1.4635);
#561=CYLINDRICAL_SURFACE('',#9895,1.4635);
#562=CYLINDRICAL_SURFACE('',#9896,1.4635);
#563=CYLINDRICAL_SURFACE('',#9897,1.4635);
#564=CYLINDRICAL_SURFACE('',#9898,1.17775);
#565=CYLINDRICAL_SURFACE('',#9900,1.17775);
#566=CYLINDRICAL_SURFACE('',#9901,1.17775);
#567=CYLINDRICAL_SURFACE('',#9902,1.17775);
#568=CYLINDRICAL_SURFACE('',#9903,1.17775);
#569=CYLINDRICAL_SURFACE('',#9904,1.17775);
#570=CYLINDRICAL_SURFACE('',#9905,1.17775);
#571=CYLINDRICAL_SURFACE('',#9906,1.17775);
#572=CYLINDRICAL_SURFACE('',#9907,1.17775);
#573=CYLINDRICAL_SURFACE('',#9908,1.17775);
#574=CYLINDRICAL_SURFACE('',#9909,1.17775);
#575=CYLINDRICAL_SURFACE('',#9910,1.17775);
#576=CYLINDRICAL_SURFACE('',#9918,1.17775);
#577=CYLINDRICAL_SURFACE('',#9931,1.4635);
#578=CYLINDRICAL_SURFACE('',#9941,2.5);
#579=FACE_BOUND('',#1377,.T.);
#580=FACE_BOUND('',#1378,.T.);
#581=FACE_BOUND('',#1379,.T.);
#582=FACE_BOUND('',#1388,.T.);
#583=FACE_BOUND('',#1389,.T.);
#584=FACE_BOUND('',#1390,.T.);
#585=FACE_BOUND('',#1422,.T.);
#586=FACE_BOUND('',#1423,.T.);
#587=FACE_BOUND('',#1424,.T.);
#588=FACE_BOUND('',#1425,.T.);
#589=FACE_BOUND('',#1426,.T.);
#590=FACE_BOUND('',#1454,.T.);
#591=FACE_BOUND('',#1455,.T.);
#592=FACE_BOUND('',#1456,.T.);
#593=FACE_BOUND('',#1457,.T.);
#594=FACE_BOUND('',#1458,.T.);
#595=FACE_BOUND('',#1459,.T.);
#596=FACE_BOUND('',#1460,.T.);
#597=FACE_BOUND('',#1461,.T.);
#598=FACE_BOUND('',#1602,.T.);
#599=FACE_BOUND('',#1603,.T.);
#600=FACE_BOUND('',#1604,.T.);
#601=FACE_BOUND('',#1605,.T.);
#602=FACE_BOUND('',#1606,.T.);
#603=FACE_BOUND('',#1609,.T.);
#604=FACE_BOUND('',#1610,.T.);
#605=FACE_BOUND('',#1611,.T.);
#606=FACE_BOUND('',#1612,.T.);
#607=FACE_BOUND('',#1613,.T.);
#608=FACE_BOUND('',#1640,.T.);
#609=FACE_BOUND('',#1641,.T.);
#610=FACE_BOUND('',#1654,.T.);
#611=FACE_BOUND('',#1655,.T.);
#612=FACE_BOUND('',#1674,.T.);
#613=FACE_BOUND('',#1675,.T.);
#614=FACE_BOUND('',#1676,.T.);
#615=FACE_BOUND('',#1724,.T.);
#616=FACE_BOUND('',#1725,.T.);
#617=FACE_BOUND('',#1726,.T.);
#618=FACE_BOUND('',#1758,.T.);
#619=FACE_BOUND('',#1765,.T.);
#620=FACE_BOUND('',#1771,.T.);
#621=FACE_BOUND('',#1775,.T.);
#622=FACE_BOUND('',#1778,.T.);
#623=FACE_BOUND('',#1792,.T.);
#624=FACE_BOUND('',#1855,.T.);
#625=FACE_BOUND('',#1857,.T.);
#626=FACE_BOUND('',#1886,.T.);
#627=FACE_BOUND('',#1924,.T.);
#628=FACE_BOUND('',#1930,.T.);
#629=CIRCLE('',#9261,2.5);
#630=CIRCLE('',#9262,2.5);
#631=CIRCLE('',#9263,2.5);
#632=CIRCLE('',#9265,14.);
#633=CIRCLE('',#9268,2.5);
#634=CIRCLE('',#9270,2.5);
#635=CIRCLE('',#9272,2.5);
#636=CIRCLE('',#9274,14.);
#637=CIRCLE('',#9296,14.);
#638=CIRCLE('',#9299,14.);
#639=CIRCLE('',#9305,4.);
#640=CIRCLE('',#9306,3.8);
#641=CIRCLE('',#9309,4.);
#642=CIRCLE('',#9310,3.8);
#643=CIRCLE('',#9313,4.);
#644=CIRCLE('',#9314,3.8);
#645=CIRCLE('',#9317,4.);
#646=CIRCLE('',#9318,3.8);
#647=CIRCLE('',#9320,4.);
#648=CIRCLE('',#9323,4.);
#649=CIRCLE('',#9326,1.7);
#650=CIRCLE('',#9327,1.7);
#651=CIRCLE('',#9328,1.7);
#652=CIRCLE('',#9329,1.7);
#653=CIRCLE('',#9330,6.5);
#654=CIRCLE('',#9333,3.85857864376269);
#655=CIRCLE('',#9336,3.85857864376269);
#656=CIRCLE('',#9339,3.85857864376269);
#657=CIRCLE('',#9340,4.);
#658=CIRCLE('',#9343,3.85857864376269);
#659=CIRCLE('',#9344,4.);
#660=CIRCLE('',#9347,3.64142135623731);
#661=CIRCLE('',#9350,3.64142135623731);
#662=CIRCLE('',#9355,3.10857864376269);
#663=CIRCLE('',#9356,3.45);
#664=CIRCLE('',#9357,3.45);
#665=CIRCLE('',#9359,3.64142135623731);
#666=CIRCLE('',#9362,1.7);
#667=CIRCLE('',#9364,3.10857864376269);
#668=CIRCLE('',#9365,3.45);
#669=CIRCLE('',#9366,3.45);
#670=CIRCLE('',#9370,1.7);
#671=CIRCLE('',#9372,3.1085786437627);
#672=CIRCLE('',#9373,3.44999999999999);
#673=CIRCLE('',#9376,3.44999999999999);
#674=CIRCLE('',#9377,6.5);
#675=CIRCLE('',#9379,1.7);
#676=CIRCLE('',#9381,3.1085786437627);
#677=CIRCLE('',#9383,1.7);
#678=CIRCLE('',#9391,3.64142135623731);
#679=CIRCLE('',#9473,4.);
#680=CIRCLE('',#9474,3.8);
#681=CIRCLE('',#9477,4.);
#682=CIRCLE('',#9478,3.8);
#683=CIRCLE('',#9481,4.);
#684=CIRCLE('',#9482,3.8);
#685=CIRCLE('',#9485,4.);
#686=CIRCLE('',#9486,3.8);
#687=CIRCLE('',#9488,4.);
#688=CIRCLE('',#9491,4.);
#689=CIRCLE('',#9494,1.7);
#690=CIRCLE('',#9495,1.7);
#691=CIRCLE('',#9496,1.7);
#692=CIRCLE('',#9497,1.7);
#693=CIRCLE('',#9498,6.5);
#694=CIRCLE('',#9500,3.1085786437627);
#695=CIRCLE('',#9501,3.44999999999999);
#696=CIRCLE('',#9503,3.8);
#697=CIRCLE('',#9504,3.8);
#698=CIRCLE('',#9505,3.8);
#699=CIRCLE('',#9506,3.8);
#700=CIRCLE('',#9507,3.45);
#701=CIRCLE('',#9508,6.5);
#702=CIRCLE('',#9509,3.44999999999999);
#703=CIRCLE('',#9510,3.45);
#704=CIRCLE('',#9512,1.7);
#705=CIRCLE('',#9515,4.);
#706=CIRCLE('',#9522,4.);
#707=CIRCLE('',#9527,3.1085786437627);
#708=CIRCLE('',#9529,1.7);
#709=CIRCLE('',#9531,3.1085786437627);
#710=CIRCLE('',#9533,1.7);
#711=CIRCLE('',#9535,3.1085786437627);
#712=CIRCLE('',#9537,1.7);
#713=CIRCLE('',#9546,2.05);
#714=CIRCLE('',#9547,1.55);
#715=CIRCLE('',#9549,14.);
#716=CIRCLE('',#9550,2.05);
#717=CIRCLE('',#9552,1.55);
#718=CIRCLE('',#9554,1.55);
#719=CIRCLE('',#9556,1.55);
#720=CIRCLE('',#9565,2.05);
#721=CIRCLE('',#9566,1.55);
#722=CIRCLE('',#9568,14.);
#723=CIRCLE('',#9569,2.05);
#724=CIRCLE('',#9571,1.55);
#725=CIRCLE('',#9573,1.55);
#726=CIRCLE('',#9575,1.55);
#727=CIRCLE('',#9595,2.5);
#728=CIRCLE('',#9596,2.5);
#729=CIRCLE('',#9597,2.5);
#730=CIRCLE('',#9645,2.5);
#731=CIRCLE('',#9646,2.5);
#732=CIRCLE('',#9647,2.5);
#733=CIRCLE('',#9666,13.4);
#734=CIRCLE('',#9668,13.9);
#735=CIRCLE('',#9670,13.9);
#736=CIRCLE('',#9672,13.4);
#737=CIRCLE('',#9676,13.4);
#738=CIRCLE('',#9677,13.9);
#739=CIRCLE('',#9678,13.9);
#740=CIRCLE('',#9680,13.9);
#741=CIRCLE('',#9684,4.5);
#742=CIRCLE('',#9685,5.);
#743=CIRCLE('',#9686,5.);
#744=CIRCLE('',#9689,5.);
#745=CIRCLE('',#9692,5.);
#746=CIRCLE('',#9694,13.4);
#747=CIRCLE('',#9698,13.9);
#748=CIRCLE('',#9699,13.9);
#749=CIRCLE('',#9700,13.55);
#750=CIRCLE('',#9703,13.9);
#751=CIRCLE('',#9705,13.4);
#752=CIRCLE('',#9707,5.);
#753=CIRCLE('',#9709,5.);
#754=CIRCLE('',#9711,4.5);
#755=CIRCLE('',#9715,8.5);
#756=CIRCLE('',#9716,8.5);
#757=CIRCLE('',#9717,8.2);
#758=CIRCLE('',#9719,5.025);
#759=CIRCLE('',#9721,8.5);
#760=CIRCLE('',#9723,5.025);
#761=CIRCLE('',#9725,6.5);
#762=CIRCLE('',#9727,6.5);
#763=CIRCLE('',#9731,4.);
#764=CIRCLE('',#9732,3.5);
#765=CIRCLE('',#9736,3.5);
#766=CIRCLE('',#9737,10.);
#767=CIRCLE('',#9739,4.);
#768=CIRCLE('',#9742,4.);
#769=CIRCLE('',#9743,3.5);
#770=CIRCLE('',#9746,10.);
#771=CIRCLE('',#9747,3.5);
#772=CIRCLE('',#9749,4.);
#773=CIRCLE('',#9757,10.);
#774=CIRCLE('',#9758,10.);
#775=CIRCLE('',#9759,10.);
#776=CIRCLE('',#9763,10.);
#777=CIRCLE('',#9765,5.025);
#778=CIRCLE('',#9793,3.5);
#779=CIRCLE('',#9794,4.);
#780=CIRCLE('',#9795,3.5);
#781=CIRCLE('',#9796,3.5);
#782=CIRCLE('',#9799,3.5);
#783=CIRCLE('',#9800,3.5);
#784=CIRCLE('',#9802,3.5);
#785=CIRCLE('',#9803,3.5);
#786=CIRCLE('',#9807,3.5);
#787=CIRCLE('',#9809,3.5);
#788=CIRCLE('',#9811,3.5);
#789=CIRCLE('',#9817,4.);
#790=CIRCLE('',#9818,3.5);
#791=CIRCLE('',#9826,4.);
#792=CIRCLE('',#9829,4.);
#793=CIRCLE('',#9835,3.5);
#794=CIRCLE('',#9843,5.025);
#795=CIRCLE('',#9845,9.5);
#796=CIRCLE('',#9849,1.954);
#797=CIRCLE('',#9855,1.5555);
#798=CIRCLE('',#9857,1.5555);
#799=CIRCLE('',#9862,1.954);
#800=CIRCLE('',#9863,1.954);
#801=CIRCLE('',#9865,1.954);
#802=CIRCLE('',#9866,1.954);
#803=CIRCLE('',#9867,1.5555);
#804=CIRCLE('',#9877,1.5);
#805=CIRCLE('',#9880,1.954);
#806=CIRCLE('',#9882,1.7);
#807=CIRCLE('',#9886,1.4635);
#808=CIRCLE('',#9899,1.17775);
#809=CIRCLE('',#9912,1.4635);
#810=CIRCLE('',#9913,1.4635);
#811=CIRCLE('',#9915,1.4635);
#812=CIRCLE('',#9916,1.4635);
#813=CIRCLE('',#9917,1.17775);
#814=CIRCLE('',#9920,0.983629653494575);
#815=CIRCLE('',#9929,1.2);
#816=CIRCLE('',#9932,1.4635);
#817=CIRCLE('',#9934,3.15);
#818=CIRCLE('',#9938,2.);
#819=CIRCLE('',#9940,2.5);
#820=CIRCLE('',#9942,2.5);
#821=CIRCLE('',#9944,2.);
#822=ELLIPSE('',#9249,19.7989898732233,14.);
#823=ELLIPSE('',#9254,19.7989898732235,14.);
#824=ELLIPSE('',#9256,19.7989898732233,14.);
#825=ELLIPSE('',#9259,19.7989898732235,14.);
#826=ELLIPSE('',#9281,19.7989898732233,14.);
#827=ELLIPSE('',#9286,19.7989898732233,14.);
#828=ELLIPSE('',#9291,19.7989898732235,14.);
#829=ELLIPSE('',#9293,19.7989898732235,14.);
#830=ELLIPSE('',#9579,19.7989898732233,14.);
#831=ELLIPSE('',#9583,19.7989898732235,14.);
#832=ELLIPSE('',#9591,19.7989898732235,14.);
#833=ELLIPSE('',#9593,19.7989898732233,14.);
#834=ELLIPSE('',#9734,14.142135623731,10.);
#835=ELLIPSE('',#9751,14.142135623731,10.);
#836=ELLIPSE('',#9754,14.142135623731,10.);
#837=ELLIPSE('',#9755,14.142135623731,10.);
#838=ELLIPSE('',#9756,14.142135623731,10.);
#839=ELLIPSE('',#9760,14.142135623731,10.);
#840=ELLIPSE('',#9761,14.142135623731,10.);
#841=ELLIPSE('',#9762,14.142135623731,10.);
#842=FACE_OUTER_BOUND('',#1364,.T.);
#843=FACE_OUTER_BOUND('',#1365,.T.);
#844=FACE_OUTER_BOUND('',#1366,.T.);
#845=FACE_OUTER_BOUND('',#1367,.T.);
#846=FACE_OUTER_BOUND('',#1368,.T.);
#847=FACE_OUTER_BOUND('',#1369,.T.);
#848=FACE_OUTER_BOUND('',#1370,.T.);
#849=FACE_OUTER_BOUND('',#1371,.T.);
#850=FACE_OUTER_BOUND('',#1372,.T.);
#851=FACE_OUTER_BOUND('',#1373,.T.);
#852=FACE_OUTER_BOUND('',#1374,.T.);
#853=FACE_OUTER_BOUND('',#1375,.T.);
#854=FACE_OUTER_BOUND('',#1376,.T.);
#855=FACE_OUTER_BOUND('',#1380,.T.);
#856=FACE_OUTER_BOUND('',#1381,.T.);
#857=FACE_OUTER_BOUND('',#1382,.T.);
#858=FACE_OUTER_BOUND('',#1383,.T.);
#859=FACE_OUTER_BOUND('',#1384,.T.);
#860=FACE_OUTER_BOUND('',#1385,.T.);
#861=FACE_OUTER_BOUND('',#1386,.T.);
#862=FACE_OUTER_BOUND('',#1387,.T.);
#863=FACE_OUTER_BOUND('',#1391,.T.);
#864=FACE_OUTER_BOUND('',#1392,.T.);
#865=FACE_OUTER_BOUND('',#1393,.T.);
#866=FACE_OUTER_BOUND('',#1394,.T.);
#867=FACE_OUTER_BOUND('',#1395,.T.);
#868=FACE_OUTER_BOUND('',#1396,.T.);
#869=FACE_OUTER_BOUND('',#1397,.T.);
#870=FACE_OUTER_BOUND('',#1398,.T.);
#871=FACE_OUTER_BOUND('',#1399,.T.);
#872=FACE_OUTER_BOUND('',#1400,.T.);
#873=FACE_OUTER_BOUND('',#1401,.T.);
#874=FACE_OUTER_BOUND('',#1402,.T.);
#875=FACE_OUTER_BOUND('',#1403,.T.);
#876=FACE_OUTER_BOUND('',#1404,.T.);
#877=FACE_OUTER_BOUND('',#1405,.T.);
#878=FACE_OUTER_BOUND('',#1406,.T.);
#879=FACE_OUTER_BOUND('',#1407,.T.);
#880=FACE_OUTER_BOUND('',#1408,.T.);
#881=FACE_OUTER_BOUND('',#1409,.T.);
#882=FACE_OUTER_BOUND('',#1410,.T.);
#883=FACE_OUTER_BOUND('',#1411,.T.);
#884=FACE_OUTER_BOUND('',#1412,.T.);
#885=FACE_OUTER_BOUND('',#1413,.T.);
#886=FACE_OUTER_BOUND('',#1414,.T.);
#887=FACE_OUTER_BOUND('',#1415,.T.);
#888=FACE_OUTER_BOUND('',#1416,.T.);
#889=FACE_OUTER_BOUND('',#1417,.T.);
#890=FACE_OUTER_BOUND('',#1418,.T.);
#891=FACE_OUTER_BOUND('',#1419,.T.);
#892=FACE_OUTER_BOUND('',#1420,.T.);
#893=FACE_OUTER_BOUND('',#1421,.T.);
#894=FACE_OUTER_BOUND('',#1427,.T.);
#895=FACE_OUTER_BOUND('',#1428,.T.);
#896=FACE_OUTER_BOUND('',#1429,.T.);
#897=FACE_OUTER_BOUND('',#1430,.T.);
#898=FACE_OUTER_BOUND('',#1431,.T.);
#899=FACE_OUTER_BOUND('',#1432,.T.);
#900=FACE_OUTER_BOUND('',#1433,.T.);
#901=FACE_OUTER_BOUND('',#1434,.T.);
#902=FACE_OUTER_BOUND('',#1435,.T.);
#903=FACE_OUTER_BOUND('',#1436,.T.);
#904=FACE_OUTER_BOUND('',#1437,.T.);
#905=FACE_OUTER_BOUND('',#1438,.T.);
#906=FACE_OUTER_BOUND('',#1439,.T.);
#907=FACE_OUTER_BOUND('',#1440,.T.);
#908=FACE_OUTER_BOUND('',#1441,.T.);
#909=FACE_OUTER_BOUND('',#1442,.T.);
#910=FACE_OUTER_BOUND('',#1443,.T.);
#911=FACE_OUTER_BOUND('',#1444,.T.);
#912=FACE_OUTER_BOUND('',#1445,.T.);
#913=FACE_OUTER_BOUND('',#1446,.T.);
#914=FACE_OUTER_BOUND('',#1447,.T.);
#915=FACE_OUTER_BOUND('',#1448,.T.);
#916=FACE_OUTER_BOUND('',#1449,.T.);
#917=FACE_OUTER_BOUND('',#1450,.T.);
#918=FACE_OUTER_BOUND('',#1451,.T.);
#919=FACE_OUTER_BOUND('',#1452,.T.);
#920=FACE_OUTER_BOUND('',#1453,.T.);
#921=FACE_OUTER_BOUND('',#1462,.T.);
#922=FACE_OUTER_BOUND('',#1463,.T.);
#923=FACE_OUTER_BOUND('',#1464,.T.);
#924=FACE_OUTER_BOUND('',#1465,.T.);
#925=FACE_OUTER_BOUND('',#1466,.T.);
#926=FACE_OUTER_BOUND('',#1467,.T.);
#927=FACE_OUTER_BOUND('',#1468,.T.);
#928=FACE_OUTER_BOUND('',#1469,.T.);
#929=FACE_OUTER_BOUND('',#1470,.T.);
#930=FACE_OUTER_BOUND('',#1471,.T.);
#931=FACE_OUTER_BOUND('',#1472,.T.);
#932=FACE_OUTER_BOUND('',#1473,.T.);
#933=FACE_OUTER_BOUND('',#1474,.T.);
#934=FACE_OUTER_BOUND('',#1475,.T.);
#935=FACE_OUTER_BOUND('',#1476,.T.);
#936=FACE_OUTER_BOUND('',#1477,.T.);
#937=FACE_OUTER_BOUND('',#1478,.T.);
#938=FACE_OUTER_BOUND('',#1479,.T.);
#939=FACE_OUTER_BOUND('',#1480,.T.);
#940=FACE_OUTER_BOUND('',#1481,.T.);
#941=FACE_OUTER_BOUND('',#1482,.T.);
#942=FACE_OUTER_BOUND('',#1483,.T.);
#943=FACE_OUTER_BOUND('',#1484,.T.);
#944=FACE_OUTER_BOUND('',#1485,.T.);
#945=FACE_OUTER_BOUND('',#1486,.T.);
#946=FACE_OUTER_BOUND('',#1487,.T.);
#947=FACE_OUTER_BOUND('',#1488,.T.);
#948=FACE_OUTER_BOUND('',#1489,.T.);
#949=FACE_OUTER_BOUND('',#1490,.T.);
#950=FACE_OUTER_BOUND('',#1491,.T.);
#951=FACE_OUTER_BOUND('',#1492,.T.);
#952=FACE_OUTER_BOUND('',#1493,.T.);
#953=FACE_OUTER_BOUND('',#1494,.T.);
#954=FACE_OUTER_BOUND('',#1495,.T.);
#955=FACE_OUTER_BOUND('',#1496,.T.);
#956=FACE_OUTER_BOUND('',#1497,.T.);
#957=FACE_OUTER_BOUND('',#1498,.T.);
#958=FACE_OUTER_BOUND('',#1499,.T.);
#959=FACE_OUTER_BOUND('',#1500,.T.);
#960=FACE_OUTER_BOUND('',#1501,.T.);
#961=FACE_OUTER_BOUND('',#1502,.T.);
#962=FACE_OUTER_BOUND('',#1503,.T.);
#963=FACE_OUTER_BOUND('',#1504,.T.);
#964=FACE_OUTER_BOUND('',#1505,.T.);
#965=FACE_OUTER_BOUND('',#1506,.T.);
#966=FACE_OUTER_BOUND('',#1507,.T.);
#967=FACE_OUTER_BOUND('',#1508,.T.);
#968=FACE_OUTER_BOUND('',#1509,.T.);
#969=FACE_OUTER_BOUND('',#1510,.T.);
#970=FACE_OUTER_BOUND('',#1511,.T.);
#971=FACE_OUTER_BOUND('',#1512,.T.);
#972=FACE_OUTER_BOUND('',#1513,.T.);
#973=FACE_OUTER_BOUND('',#1514,.T.);
#974=FACE_OUTER_BOUND('',#1515,.T.);
#975=FACE_OUTER_BOUND('',#1516,.T.);
#976=FACE_OUTER_BOUND('',#1517,.T.);
#977=FACE_OUTER_BOUND('',#1518,.T.);
#978=FACE_OUTER_BOUND('',#1519,.T.);
#979=FACE_OUTER_BOUND('',#1520,.T.);
#980=FACE_OUTER_BOUND('',#1521,.T.);
#981=FACE_OUTER_BOUND('',#1522,.T.);
#982=FACE_OUTER_BOUND('',#1523,.T.);
#983=FACE_OUTER_BOUND('',#1524,.T.);
#984=FACE_OUTER_BOUND('',#1525,.T.);
#985=FACE_OUTER_BOUND('',#1526,.T.);
#986=FACE_OUTER_BOUND('',#1527,.T.);
#987=FACE_OUTER_BOUND('',#1528,.T.);
#988=FACE_OUTER_BOUND('',#1529,.T.);
#989=FACE_OUTER_BOUND('',#1530,.T.);
#990=FACE_OUTER_BOUND('',#1531,.T.);
#991=FACE_OUTER_BOUND('',#1532,.T.);
#992=FACE_OUTER_BOUND('',#1533,.T.);
#993=FACE_OUTER_BOUND('',#1534,.T.);
#994=FACE_OUTER_BOUND('',#1535,.T.);
#995=FACE_OUTER_BOUND('',#1536,.T.);
#996=FACE_OUTER_BOUND('',#1537,.T.);
#997=FACE_OUTER_BOUND('',#1538,.T.);
#998=FACE_OUTER_BOUND('',#1539,.T.);
#999=FACE_OUTER_BOUND('',#1540,.T.);
#1000=FACE_OUTER_BOUND('',#1541,.T.);
#1001=FACE_OUTER_BOUND('',#1542,.T.);
#1002=FACE_OUTER_BOUND('',#1543,.T.);
#1003=FACE_OUTER_BOUND('',#1544,.T.);
#1004=FACE_OUTER_BOUND('',#1545,.T.);
#1005=FACE_OUTER_BOUND('',#1546,.T.);
#1006=FACE_OUTER_BOUND('',#1547,.T.);
#1007=FACE_OUTER_BOUND('',#1548,.T.);
#1008=FACE_OUTER_BOUND('',#1549,.T.);
#1009=FACE_OUTER_BOUND('',#1550,.T.);
#1010=FACE_OUTER_BOUND('',#1551,.T.);
#1011=FACE_OUTER_BOUND('',#1552,.T.);
#1012=FACE_OUTER_BOUND('',#1553,.T.);
#1013=FACE_OUTER_BOUND('',#1554,.T.);
#1014=FACE_OUTER_BOUND('',#1555,.T.);
#1015=FACE_OUTER_BOUND('',#1556,.T.);
#1016=FACE_OUTER_BOUND('',#1557,.T.);
#1017=FACE_OUTER_BOUND('',#1558,.T.);
#1018=FACE_OUTER_BOUND('',#1559,.T.);
#1019=FACE_OUTER_BOUND('',#1560,.T.);
#1020=FACE_OUTER_BOUND('',#1561,.T.);
#1021=FACE_OUTER_BOUND('',#1562,.T.);
#1022=FACE_OUTER_BOUND('',#1563,.T.);
#1023=FACE_OUTER_BOUND('',#1564,.T.);
#1024=FACE_OUTER_BOUND('',#1565,.T.);
#1025=FACE_OUTER_BOUND('',#1566,.T.);
#1026=FACE_OUTER_BOUND('',#1567,.T.);
#1027=FACE_OUTER_BOUND('',#1568,.T.);
#1028=FACE_OUTER_BOUND('',#1569,.T.);
#1029=FACE_OUTER_BOUND('',#1570,.T.);
#1030=FACE_OUTER_BOUND('',#1571,.T.);
#1031=FACE_OUTER_BOUND('',#1572,.T.);
#1032=FACE_OUTER_BOUND('',#1573,.T.);
#1033=FACE_OUTER_BOUND('',#1574,.T.);
#1034=FACE_OUTER_BOUND('',#1575,.T.);
#1035=FACE_OUTER_BOUND('',#1576,.T.);
#1036=FACE_OUTER_BOUND('',#1577,.T.);
#1037=FACE_OUTER_BOUND('',#1578,.T.);
#1038=FACE_OUTER_BOUND('',#1579,.T.);
#1039=FACE_OUTER_BOUND('',#1580,.T.);
#1040=FACE_OUTER_BOUND('',#1581,.T.);
#1041=FACE_OUTER_BOUND('',#1582,.T.);
#1042=FACE_OUTER_BOUND('',#1583,.T.);
#1043=FACE_OUTER_BOUND('',#1584,.T.);
#1044=FACE_OUTER_BOUND('',#1585,.T.);
#1045=FACE_OUTER_BOUND('',#1586,.T.);
#1046=FACE_OUTER_BOUND('',#1587,.T.);
#1047=FACE_OUTER_BOUND('',#1588,.T.);
#1048=FACE_OUTER_BOUND('',#1589,.T.);
#1049=FACE_OUTER_BOUND('',#1590,.T.);
#1050=FACE_OUTER_BOUND('',#1591,.T.);
#1051=FACE_OUTER_BOUND('',#1592,.T.);
#1052=FACE_OUTER_BOUND('',#1593,.T.);
#1053=FACE_OUTER_BOUND('',#1594,.T.);
#1054=FACE_OUTER_BOUND('',#1595,.T.);
#1055=FACE_OUTER_BOUND('',#1596,.T.);
#1056=FACE_OUTER_BOUND('',#1597,.T.);
#1057=FACE_OUTER_BOUND('',#1598,.T.);
#1058=FACE_OUTER_BOUND('',#1599,.T.);
#1059=FACE_OUTER_BOUND('',#1600,.T.);
#1060=FACE_OUTER_BOUND('',#1601,.T.);
#1061=FACE_OUTER_BOUND('',#1607,.T.);
#1062=FACE_OUTER_BOUND('',#1608,.T.);
#1063=FACE_OUTER_BOUND('',#1614,.T.);
#1064=FACE_OUTER_BOUND('',#1615,.T.);
#1065=FACE_OUTER_BOUND('',#1616,.T.);
#1066=FACE_OUTER_BOUND('',#1617,.T.);
#1067=FACE_OUTER_BOUND('',#1618,.T.);
#1068=FACE_OUTER_BOUND('',#1619,.T.);
#1069=FACE_OUTER_BOUND('',#1620,.T.);
#1070=FACE_OUTER_BOUND('',#1621,.T.);
#1071=FACE_OUTER_BOUND('',#1622,.T.);
#1072=FACE_OUTER_BOUND('',#1623,.T.);
#1073=FACE_OUTER_BOUND('',#1624,.T.);
#1074=FACE_OUTER_BOUND('',#1625,.T.);
#1075=FACE_OUTER_BOUND('',#1626,.T.);
#1076=FACE_OUTER_BOUND('',#1627,.T.);
#1077=FACE_OUTER_BOUND('',#1628,.T.);
#1078=FACE_OUTER_BOUND('',#1629,.T.);
#1079=FACE_OUTER_BOUND('',#1630,.T.);
#1080=FACE_OUTER_BOUND('',#1631,.T.);
#1081=FACE_OUTER_BOUND('',#1632,.T.);
#1082=FACE_OUTER_BOUND('',#1633,.T.);
#1083=FACE_OUTER_BOUND('',#1634,.T.);
#1084=FACE_OUTER_BOUND('',#1635,.T.);
#1085=FACE_OUTER_BOUND('',#1636,.T.);
#1086=FACE_OUTER_BOUND('',#1637,.T.);
#1087=FACE_OUTER_BOUND('',#1638,.T.);
#1088=FACE_OUTER_BOUND('',#1639,.T.);
#1089=FACE_OUTER_BOUND('',#1642,.T.);
#1090=FACE_OUTER_BOUND('',#1643,.T.);
#1091=FACE_OUTER_BOUND('',#1644,.T.);
#1092=FACE_OUTER_BOUND('',#1645,.T.);
#1093=FACE_OUTER_BOUND('',#1646,.T.);
#1094=FACE_OUTER_BOUND('',#1647,.T.);
#1095=FACE_OUTER_BOUND('',#1648,.T.);
#1096=FACE_OUTER_BOUND('',#1649,.T.);
#1097=FACE_OUTER_BOUND('',#1650,.T.);
#1098=FACE_OUTER_BOUND('',#1651,.T.);
#1099=FACE_OUTER_BOUND('',#1652,.T.);
#1100=FACE_OUTER_BOUND('',#1653,.T.);
#1101=FACE_OUTER_BOUND('',#1656,.T.);
#1102=FACE_OUTER_BOUND('',#1657,.T.);
#1103=FACE_OUTER_BOUND('',#1658,.T.);
#1104=FACE_OUTER_BOUND('',#1659,.T.);
#1105=FACE_OUTER_BOUND('',#1660,.T.);
#1106=FACE_OUTER_BOUND('',#1661,.T.);
#1107=FACE_OUTER_BOUND('',#1662,.T.);
#1108=FACE_OUTER_BOUND('',#1663,.T.);
#1109=FACE_OUTER_BOUND('',#1664,.T.);
#1110=FACE_OUTER_BOUND('',#1665,.T.);
#1111=FACE_OUTER_BOUND('',#1666,.T.);
#1112=FACE_OUTER_BOUND('',#1667,.T.);
#1113=FACE_OUTER_BOUND('',#1668,.T.);
#1114=FACE_OUTER_BOUND('',#1669,.T.);
#1115=FACE_OUTER_BOUND('',#1670,.T.);
#1116=FACE_OUTER_BOUND('',#1671,.T.);
#1117=FACE_OUTER_BOUND('',#1672,.T.);
#1118=FACE_OUTER_BOUND('',#1673,.T.);
#1119=FACE_OUTER_BOUND('',#1677,.T.);
#1120=FACE_OUTER_BOUND('',#1678,.T.);
#1121=FACE_OUTER_BOUND('',#1679,.T.);
#1122=FACE_OUTER_BOUND('',#1680,.T.);
#1123=FACE_OUTER_BOUND('',#1681,.T.);
#1124=FACE_OUTER_BOUND('',#1682,.T.);
#1125=FACE_OUTER_BOUND('',#1683,.T.);
#1126=FACE_OUTER_BOUND('',#1684,.T.);
#1127=FACE_OUTER_BOUND('',#1685,.T.);
#1128=FACE_OUTER_BOUND('',#1686,.T.);
#1129=FACE_OUTER_BOUND('',#1687,.T.);
#1130=FACE_OUTER_BOUND('',#1688,.T.);
#1131=FACE_OUTER_BOUND('',#1689,.T.);
#1132=FACE_OUTER_BOUND('',#1690,.T.);
#1133=FACE_OUTER_BOUND('',#1691,.T.);
#1134=FACE_OUTER_BOUND('',#1692,.T.);
#1135=FACE_OUTER_BOUND('',#1693,.T.);
#1136=FACE_OUTER_BOUND('',#1694,.T.);
#1137=FACE_OUTER_BOUND('',#1695,.T.);
#1138=FACE_OUTER_BOUND('',#1696,.T.);
#1139=FACE_OUTER_BOUND('',#1697,.T.);
#1140=FACE_OUTER_BOUND('',#1698,.T.);
#1141=FACE_OUTER_BOUND('',#1699,.T.);
#1142=FACE_OUTER_BOUND('',#1700,.T.);
#1143=FACE_OUTER_BOUND('',#1701,.T.);
#1144=FACE_OUTER_BOUND('',#1702,.T.);
#1145=FACE_OUTER_BOUND('',#1703,.T.);
#1146=FACE_OUTER_BOUND('',#1704,.T.);
#1147=FACE_OUTER_BOUND('',#1705,.T.);
#1148=FACE_OUTER_BOUND('',#1706,.T.);
#1149=FACE_OUTER_BOUND('',#1707,.T.);
#1150=FACE_OUTER_BOUND('',#1708,.T.);
#1151=FACE_OUTER_BOUND('',#1709,.T.);
#1152=FACE_OUTER_BOUND('',#1710,.T.);
#1153=FACE_OUTER_BOUND('',#1711,.T.);
#1154=FACE_OUTER_BOUND('',#1712,.T.);
#1155=FACE_OUTER_BOUND('',#1713,.T.);
#1156=FACE_OUTER_BOUND('',#1714,.T.);
#1157=FACE_OUTER_BOUND('',#1715,.T.);
#1158=FACE_OUTER_BOUND('',#1716,.T.);
#1159=FACE_OUTER_BOUND('',#1717,.T.);
#1160=FACE_OUTER_BOUND('',#1718,.T.);
#1161=FACE_OUTER_BOUND('',#1719,.T.);
#1162=FACE_OUTER_BOUND('',#1720,.T.);
#1163=FACE_OUTER_BOUND('',#1721,.T.);
#1164=FACE_OUTER_BOUND('',#1722,.T.);
#1165=FACE_OUTER_BOUND('',#1723,.T.);
#1166=FACE_OUTER_BOUND('',#1727,.T.);
#1167=FACE_OUTER_BOUND('',#1728,.T.);
#1168=FACE_OUTER_BOUND('',#1729,.T.);
#1169=FACE_OUTER_BOUND('',#1730,.T.);
#1170=FACE_OUTER_BOUND('',#1731,.T.);
#1171=FACE_OUTER_BOUND('',#1732,.T.);
#1172=FACE_OUTER_BOUND('',#1733,.T.);
#1173=FACE_OUTER_BOUND('',#1734,.T.);
#1174=FACE_OUTER_BOUND('',#1735,.T.);
#1175=FACE_OUTER_BOUND('',#1736,.T.);
#1176=FACE_OUTER_BOUND('',#1737,.T.);
#1177=FACE_OUTER_BOUND('',#1738,.T.);
#1178=FACE_OUTER_BOUND('',#1739,.T.);
#1179=FACE_OUTER_BOUND('',#1740,.T.);
#1180=FACE_OUTER_BOUND('',#1741,.T.);
#1181=FACE_OUTER_BOUND('',#1742,.T.);
#1182=FACE_OUTER_BOUND('',#1743,.T.);
#1183=FACE_OUTER_BOUND('',#1744,.T.);
#1184=FACE_OUTER_BOUND('',#1745,.T.);
#1185=FACE_OUTER_BOUND('',#1746,.T.);
#1186=FACE_OUTER_BOUND('',#1747,.T.);
#1187=FACE_OUTER_BOUND('',#1748,.T.);
#1188=FACE_OUTER_BOUND('',#1749,.T.);
#1189=FACE_OUTER_BOUND('',#1750,.T.);
#1190=FACE_OUTER_BOUND('',#1751,.T.);
#1191=FACE_OUTER_BOUND('',#1752,.T.);
#1192=FACE_OUTER_BOUND('',#1753,.T.);
#1193=FACE_OUTER_BOUND('',#1754,.T.);
#1194=FACE_OUTER_BOUND('',#1755,.T.);
#1195=FACE_OUTER_BOUND('',#1756,.T.);
#1196=FACE_OUTER_BOUND('',#1757,.T.);
#1197=FACE_OUTER_BOUND('',#1759,.T.);
#1198=FACE_OUTER_BOUND('',#1760,.T.);
#1199=FACE_OUTER_BOUND('',#1761,.T.);
#1200=FACE_OUTER_BOUND('',#1762,.T.);
#1201=FACE_OUTER_BOUND('',#1763,.T.);
#1202=FACE_OUTER_BOUND('',#1764,.T.);
#1203=FACE_OUTER_BOUND('',#1766,.T.);
#1204=FACE_OUTER_BOUND('',#1767,.T.);
#1205=FACE_OUTER_BOUND('',#1768,.T.);
#1206=FACE_OUTER_BOUND('',#1769,.T.);
#1207=FACE_OUTER_BOUND('',#1770,.T.);
#1208=FACE_OUTER_BOUND('',#1772,.T.);
#1209=FACE_OUTER_BOUND('',#1773,.T.);
#1210=FACE_OUTER_BOUND('',#1774,.T.);
#1211=FACE_OUTER_BOUND('',#1776,.T.);
#1212=FACE_OUTER_BOUND('',#1777,.T.);
#1213=FACE_OUTER_BOUND('',#1779,.T.);
#1214=FACE_OUTER_BOUND('',#1780,.T.);
#1215=FACE_OUTER_BOUND('',#1781,.T.);
#1216=FACE_OUTER_BOUND('',#1782,.T.);
#1217=FACE_OUTER_BOUND('',#1783,.T.);
#1218=FACE_OUTER_BOUND('',#1784,.T.);
#1219=FACE_OUTER_BOUND('',#1785,.T.);
#1220=FACE_OUTER_BOUND('',#1786,.T.);
#1221=FACE_OUTER_BOUND('',#1787,.T.);
#1222=FACE_OUTER_BOUND('',#1788,.T.);
#1223=FACE_OUTER_BOUND('',#1789,.T.);
#1224=FACE_OUTER_BOUND('',#1790,.T.);
#1225=FACE_OUTER_BOUND('',#1791,.T.);
#1226=FACE_OUTER_BOUND('',#1793,.T.);
#1227=FACE_OUTER_BOUND('',#1794,.T.);
#1228=FACE_OUTER_BOUND('',#1795,.T.);
#1229=FACE_OUTER_BOUND('',#1796,.T.);
#1230=FACE_OUTER_BOUND('',#1797,.T.);
#1231=FACE_OUTER_BOUND('',#1798,.T.);
#1232=FACE_OUTER_BOUND('',#1799,.T.);
#1233=FACE_OUTER_BOUND('',#1800,.T.);
#1234=FACE_OUTER_BOUND('',#1801,.T.);
#1235=FACE_OUTER_BOUND('',#1802,.T.);
#1236=FACE_OUTER_BOUND('',#1803,.T.);
#1237=FACE_OUTER_BOUND('',#1804,.T.);
#1238=FACE_OUTER_BOUND('',#1805,.T.);
#1239=FACE_OUTER_BOUND('',#1806,.T.);
#1240=FACE_OUTER_BOUND('',#1807,.T.);
#1241=FACE_OUTER_BOUND('',#1808,.T.);
#1242=FACE_OUTER_BOUND('',#1809,.T.);
#1243=FACE_OUTER_BOUND('',#1810,.T.);
#1244=FACE_OUTER_BOUND('',#1811,.T.);
#1245=FACE_OUTER_BOUND('',#1812,.T.);
#1246=FACE_OUTER_BOUND('',#1813,.T.);
#1247=FACE_OUTER_BOUND('',#1814,.T.);
#1248=FACE_OUTER_BOUND('',#1815,.T.);
#1249=FACE_OUTER_BOUND('',#1816,.T.);
#1250=FACE_OUTER_BOUND('',#1817,.T.);
#1251=FACE_OUTER_BOUND('',#1818,.T.);
#1252=FACE_OUTER_BOUND('',#1819,.T.);
#1253=FACE_OUTER_BOUND('',#1820,.T.);
#1254=FACE_OUTER_BOUND('',#1821,.T.);
#1255=FACE_OUTER_BOUND('',#1822,.T.);
#1256=FACE_OUTER_BOUND('',#1823,.T.);
#1257=FACE_OUTER_BOUND('',#1824,.T.);
#1258=FACE_OUTER_BOUND('',#1825,.T.);
#1259=FACE_OUTER_BOUND('',#1826,.T.);
#1260=FACE_OUTER_BOUND('',#1827,.T.);
#1261=FACE_OUTER_BOUND('',#1828,.T.);
#1262=FACE_OUTER_BOUND('',#1829,.T.);
#1263=FACE_OUTER_BOUND('',#1830,.T.);
#1264=FACE_OUTER_BOUND('',#1831,.T.);
#1265=FACE_OUTER_BOUND('',#1832,.T.);
#1266=FACE_OUTER_BOUND('',#1833,.T.);
#1267=FACE_OUTER_BOUND('',#1834,.T.);
#1268=FACE_OUTER_BOUND('',#1835,.T.);
#1269=FACE_OUTER_BOUND('',#1836,.T.);
#1270=FACE_OUTER_BOUND('',#1837,.T.);
#1271=FACE_OUTER_BOUND('',#1838,.T.);
#1272=FACE_OUTER_BOUND('',#1839,.T.);
#1273=FACE_OUTER_BOUND('',#1840,.T.);
#1274=FACE_OUTER_BOUND('',#1841,.T.);
#1275=FACE_OUTER_BOUND('',#1842,.T.);
#1276=FACE_OUTER_BOUND('',#1843,.T.);
#1277=FACE_OUTER_BOUND('',#1844,.T.);
#1278=FACE_OUTER_BOUND('',#1845,.T.);
#1279=FACE_OUTER_BOUND('',#1846,.T.);
#1280=FACE_OUTER_BOUND('',#1847,.T.);
#1281=FACE_OUTER_BOUND('',#1848,.T.);
#1282=FACE_OUTER_BOUND('',#1849,.T.);
#1283=FACE_OUTER_BOUND('',#1850,.T.);
#1284=FACE_OUTER_BOUND('',#1851,.T.);
#1285=FACE_OUTER_BOUND('',#1852,.T.);
#1286=FACE_OUTER_BOUND('',#1853,.T.);
#1287=FACE_OUTER_BOUND('',#1854,.T.);
#1288=FACE_OUTER_BOUND('',#1856,.T.);
#1289=FACE_OUTER_BOUND('',#1858,.T.);
#1290=FACE_OUTER_BOUND('',#1859,.T.);
#1291=FACE_OUTER_BOUND('',#1860,.T.);
#1292=FACE_OUTER_BOUND('',#1861,.T.);
#1293=FACE_OUTER_BOUND('',#1862,.T.);
#1294=FACE_OUTER_BOUND('',#1863,.T.);
#1295=FACE_OUTER_BOUND('',#1864,.T.);
#1296=FACE_OUTER_BOUND('',#1865,.T.);
#1297=FACE_OUTER_BOUND('',#1866,.T.);
#1298=FACE_OUTER_BOUND('',#1867,.T.);
#1299=FACE_OUTER_BOUND('',#1868,.T.);
#1300=FACE_OUTER_BOUND('',#1869,.T.);
#1301=FACE_OUTER_BOUND('',#1870,.T.);
#1302=FACE_OUTER_BOUND('',#1871,.T.);
#1303=FACE_OUTER_BOUND('',#1872,.T.);
#1304=FACE_OUTER_BOUND('',#1873,.T.);
#1305=FACE_OUTER_BOUND('',#1874,.T.);
#1306=FACE_OUTER_BOUND('',#1875,.T.);
#1307=FACE_OUTER_BOUND('',#1876,.T.);
#1308=FACE_OUTER_BOUND('',#1877,.T.);
#1309=FACE_OUTER_BOUND('',#1878,.T.);
#1310=FACE_OUTER_BOUND('',#1879,.T.);
#1311=FACE_OUTER_BOUND('',#1880,.T.);
#1312=FACE_OUTER_BOUND('',#1881,.T.);
#1313=FACE_OUTER_BOUND('',#1882,.T.);
#1314=FACE_OUTER_BOUND('',#1883,.T.);
#1315=FACE_OUTER_BOUND('',#1884,.T.);
#1316=FACE_OUTER_BOUND('',#1885,.T.);
#1317=FACE_OUTER_BOUND('',#1887,.T.);
#1318=FACE_OUTER_BOUND('',#1888,.T.);
#1319=FACE_OUTER_BOUND('',#1889,.T.);
#1320=FACE_OUTER_BOUND('',#1890,.T.);
#1321=FACE_OUTER_BOUND('',#1891,.T.);
#1322=FACE_OUTER_BOUND('',#1892,.T.);
#1323=FACE_OUTER_BOUND('',#1893,.T.);
#1324=FACE_OUTER_BOUND('',#1894,.T.);
#1325=FACE_OUTER_BOUND('',#1895,.T.);
#1326=FACE_OUTER_BOUND('',#1896,.T.);
#1327=FACE_OUTER_BOUND('',#1897,.T.);
#1328=FACE_OUTER_BOUND('',#1898,.T.);
#1329=FACE_OUTER_BOUND('',#1899,.T.);
#1330=FACE_OUTER_BOUND('',#1900,.T.);
#1331=FACE_OUTER_BOUND('',#1901,.T.);
#1332=FACE_OUTER_BOUND('',#1902,.T.);
#1333=FACE_OUTER_BOUND('',#1903,.T.);
#1334=FACE_OUTER_BOUND('',#1904,.T.);
#1335=FACE_OUTER_BOUND('',#1905,.T.);
#1336=FACE_OUTER_BOUND('',#1906,.T.);
#1337=FACE_OUTER_BOUND('',#1907,.T.);
#1338=FACE_OUTER_BOUND('',#1908,.T.);
#1339=FACE_OUTER_BOUND('',#1909,.T.);
#1340=FACE_OUTER_BOUND('',#1910,.T.);
#1341=FACE_OUTER_BOUND('',#1911,.T.);
#1342=FACE_OUTER_BOUND('',#1912,.T.);
#1343=FACE_OUTER_BOUND('',#1913,.T.);
#1344=FACE_OUTER_BOUND('',#1914,.T.);
#1345=FACE_OUTER_BOUND('',#1915,.T.);
#1346=FACE_OUTER_BOUND('',#1916,.T.);
#1347=FACE_OUTER_BOUND('',#1917,.T.);
#1348=FACE_OUTER_BOUND('',#1918,.T.);
#1349=FACE_OUTER_BOUND('',#1919,.T.);
#1350=FACE_OUTER_BOUND('',#1920,.T.);
#1351=FACE_OUTER_BOUND('',#1921,.T.);
#1352=FACE_OUTER_BOUND('',#1922,.T.);
#1353=FACE_OUTER_BOUND('',#1923,.T.);
#1354=FACE_OUTER_BOUND('',#1925,.T.);
#1355=FACE_OUTER_BOUND('',#1926,.T.);
#1356=FACE_OUTER_BOUND('',#1927,.T.);
#1357=FACE_OUTER_BOUND('',#1928,.T.);
#1358=FACE_OUTER_BOUND('',#1929,.T.);
#1359=FACE_OUTER_BOUND('',#1931,.T.);
#1360=FACE_OUTER_BOUND('',#1932,.T.);
#1361=FACE_OUTER_BOUND('',#1933,.T.);
#1362=FACE_OUTER_BOUND('',#1934,.T.);
#1363=FACE_OUTER_BOUND('',#1935,.T.);
#1364=EDGE_LOOP('',(#5692,#5693,#5694));
#1365=EDGE_LOOP('',(#5695,#5696,#5697));
#1366=EDGE_LOOP('',(#5698,#5699,#5700));
#1367=EDGE_LOOP('',(#5701,#5702,#5703));
#1368=EDGE_LOOP('',(#5704,#5705,#5706,#5707));
#1369=EDGE_LOOP('',(#5708,#5709,#5710,#5711));
#1370=EDGE_LOOP('',(#5712,#5713,#5714,#5715));
#1371=EDGE_LOOP('',(#5716,#5717,#5718,#5719));
#1372=EDGE_LOOP('',(#5720,#5721,#5722,#5723));
#1373=EDGE_LOOP('',(#5724,#5725,#5726,#5727));
#1374=EDGE_LOOP('',(#5728,#5729,#5730,#5731));
#1375=EDGE_LOOP('',(#5732,#5733,#5734,#5735));
#1376=EDGE_LOOP('',(#5736,#5737,#5738,#5739));
#1377=EDGE_LOOP('',(#5740));
#1378=EDGE_LOOP('',(#5741));
#1379=EDGE_LOOP('',(#5742));
#1380=EDGE_LOOP('',(#5743,#5744,#5745,#5746));
#1381=EDGE_LOOP('',(#5747,#5748,#5749,#5750));
#1382=EDGE_LOOP('',(#5751,#5752,#5753,#5754));
#1383=EDGE_LOOP('',(#5755,#5756,#5757,#5758));
#1384=EDGE_LOOP('',(#5759,#5760,#5761,#5762));
#1385=EDGE_LOOP('',(#5763,#5764,#5765,#5766,#5767,#5768,#5769,#5770));
#1386=EDGE_LOOP('',(#5771,#5772,#5773,#5774));
#1387=EDGE_LOOP('',(#5775,#5776,#5777,#5778));
#1388=EDGE_LOOP('',(#5779));
#1389=EDGE_LOOP('',(#5780));
#1390=EDGE_LOOP('',(#5781));
#1391=EDGE_LOOP('',(#5782,#5783,#5784));
#1392=EDGE_LOOP('',(#5785,#5786,#5787));
#1393=EDGE_LOOP('',(#5788,#5789,#5790,#5791));
#1394=EDGE_LOOP('',(#5792,#5793,#5794,#5795));
#1395=EDGE_LOOP('',(#5796,#5797,#5798));
#1396=EDGE_LOOP('',(#5799,#5800,#5801));
#1397=EDGE_LOOP('',(#5802,#5803,#5804,#5805));
#1398=EDGE_LOOP('',(#5806,#5807,#5808,#5809));
#1399=EDGE_LOOP('',(#5810,#5811,#5812,#5813));
#1400=EDGE_LOOP('',(#5814,#5815,#5816,#5817));
#1401=EDGE_LOOP('',(#5818,#5819,#5820,#5821));
#1402=EDGE_LOOP('',(#5822,#5823,#5824,#5825));
#1403=EDGE_LOOP('',(#5826,#5827,#5828,#5829));
#1404=EDGE_LOOP('',(#5830,#5831,#5832,#5833));
#1405=EDGE_LOOP('',(#5834,#5835,#5836,#5837));
#1406=EDGE_LOOP('',(#5838,#5839,#5840,#5841,#5842,#5843,#5844,#5845));
#1407=EDGE_LOOP('',(#5846,#5847,#5848,#5849));
#1408=EDGE_LOOP('',(#5850,#5851,#5852,#5853));
#1409=EDGE_LOOP('',(#5854,#5855,#5856,#5857));
#1410=EDGE_LOOP('',(#5858,#5859,#5860,#5861));
#1411=EDGE_LOOP('',(#5862,#5863,#5864,#5865));
#1412=EDGE_LOOP('',(#5866,#5867,#5868,#5869));
#1413=EDGE_LOOP('',(#5870,#5871,#5872,#5873));
#1414=EDGE_LOOP('',(#5874,#5875,#5876,#5877));
#1415=EDGE_LOOP('',(#5878,#5879,#5880,#5881));
#1416=EDGE_LOOP('',(#5882,#5883,#5884,#5885));
#1417=EDGE_LOOP('',(#5886,#5887,#5888,#5889));
#1418=EDGE_LOOP('',(#5890,#5891,#5892,#5893));
#1419=EDGE_LOOP('',(#5894,#5895,#5896,#5897));
#1420=EDGE_LOOP('',(#5898,#5899,#5900,#5901));
#1421=EDGE_LOOP('',(#5902,#5903,#5904,#5905,#5906,#5907,#5908,#5909));
#1422=EDGE_LOOP('',(#5910));
#1423=EDGE_LOOP('',(#5911));
#1424=EDGE_LOOP('',(#5912));
#1425=EDGE_LOOP('',(#5913));
#1426=EDGE_LOOP('',(#5914));
#1427=EDGE_LOOP('',(#5915,#5916,#5917,#5918));
#1428=EDGE_LOOP('',(#5919,#5920,#5921,#5922));
#1429=EDGE_LOOP('',(#5923,#5924,#5925,#5926));
#1430=EDGE_LOOP('',(#5927,#5928,#5929,#5930));
#1431=EDGE_LOOP('',(#5931,#5932,#5933,#5934));
#1432=EDGE_LOOP('',(#5935,#5936,#5937,#5938));
#1433=EDGE_LOOP('',(#5939,#5940,#5941,#5942,#5943,#5944,#5945,#5946));
#1434=EDGE_LOOP('',(#5947,#5948,#5949,#5950));
#1435=EDGE_LOOP('',(#5951,#5952,#5953,#5954));
#1436=EDGE_LOOP('',(#5955,#5956,#5957,#5958));
#1437=EDGE_LOOP('',(#5959,#5960,#5961,#5962));
#1438=EDGE_LOOP('',(#5963,#5964,#5965,#5966));
#1439=EDGE_LOOP('',(#5967,#5968,#5969,#5970,#5971,#5972,#5973,#5974,#5975,
#5976,#5977,#5978,#5979));
#1440=EDGE_LOOP('',(#5980,#5981,#5982,#5983,#5984));
#1441=EDGE_LOOP('',(#5985,#5986,#5987,#5988,#5989,#5990,#5991,#5992));
#1442=EDGE_LOOP('',(#5993,#5994,#5995,#5996));
#1443=EDGE_LOOP('',(#5997,#5998,#5999,#6000,#6001,#6002,#6003,#6004));
#1444=EDGE_LOOP('',(#6005,#6006,#6007,#6008));
#1445=EDGE_LOOP('',(#6009,#6010,#6011,#6012,#6013,#6014,#6015));
#1446=EDGE_LOOP('',(#6016,#6017,#6018,#6019));
#1447=EDGE_LOOP('',(#6020,#6021,#6022,#6023,#6024,#6025,#6026,#6027));
#1448=EDGE_LOOP('',(#6028,#6029,#6030,#6031));
#1449=EDGE_LOOP('',(#6032,#6033,#6034,#6035,#6036,#6037));
#1450=EDGE_LOOP('',(#6038,#6039,#6040,#6041));
#1451=EDGE_LOOP('',(#6042,#6043,#6044,#6045,#6046,#6047,#6048,#6049));
#1452=EDGE_LOOP('',(#6050,#6051,#6052,#6053,#6054,#6055));
#1453=EDGE_LOOP('',(#6056,#6057,#6058,#6059,#6060,#6061,#6062,#6063,#6064,
#6065,#6066,#6067,#6068,#6069,#6070,#6071,#6072,#6073,#6074,#6075,#6076,
#6077,#6078,#6079,#6080,#6081,#6082,#6083,#6084,#6085,#6086,#6087,#6088,
#6089));
#1454=EDGE_LOOP('',(#6090,#6091,#6092,#6093,#6094,#6095,#6096,#6097,#6098,
#6099));
#1455=EDGE_LOOP('',(#6100,#6101,#6102,#6103,#6104,#6105,#6106,#6107,#6108,
#6109));
#1456=EDGE_LOOP('',(#6110,#6111,#6112,#6113,#6114,#6115,#6116,#6117,#6118,
#6119,#6120));
#1457=EDGE_LOOP('',(#6121,#6122,#6123,#6124,#6125,#6126,#6127,#6128,#6129,
#6130));
#1458=EDGE_LOOP('',(#6131,#6132,#6133,#6134,#6135,#6136,#6137,#6138,#6139,
#6140,#6141));
#1459=EDGE_LOOP('',(#6142));
#1460=EDGE_LOOP('',(#6143,#6144,#6145,#6146,#6147,#6148,#6149,#6150,#6151,
#6152,#6153));
#1461=EDGE_LOOP('',(#6154,#6155,#6156,#6157,#6158,#6159,#6160,#6161,#6162,
#6163));
#1462=EDGE_LOOP('',(#6164,#6165,#6166,#6167));
#1463=EDGE_LOOP('',(#6168,#6169,#6170,#6171,#6172,#6173,#6174,#6175));
#1464=EDGE_LOOP('',(#6176,#6177,#6178,#6179));
#1465=EDGE_LOOP('',(#6180,#6181,#6182,#6183,#6184,#6185));
#1466=EDGE_LOOP('',(#6186,#6187,#6188,#6189));
#1467=EDGE_LOOP('',(#6190,#6191,#6192,#6193));
#1468=EDGE_LOOP('',(#6194,#6195,#6196,#6197,#6198));
#1469=EDGE_LOOP('',(#6199,#6200,#6201,#6202));
#1470=EDGE_LOOP('',(#6203,#6204,#6205,#6206,#6207,#6208,#6209,#6210));
#1471=EDGE_LOOP('',(#6211,#6212,#6213,#6214));
#1472=EDGE_LOOP('',(#6215,#6216,#6217,#6218));
#1473=EDGE_LOOP('',(#6219,#6220,#6221,#6222));
#1474=EDGE_LOOP('',(#6223,#6224,#6225,#6226));
#1475=EDGE_LOOP('',(#6227,#6228,#6229,#6230));
#1476=EDGE_LOOP('',(#6231,#6232,#6233,#6234));
#1477=EDGE_LOOP('',(#6235,#6236,#6237,#6238));
#1478=EDGE_LOOP('',(#6239,#6240,#6241,#6242,#6243,#6244,#6245,#6246));
#1479=EDGE_LOOP('',(#6247,#6248,#6249,#6250,#6251));
#1480=EDGE_LOOP('',(#6252,#6253,#6254,#6255));
#1481=EDGE_LOOP('',(#6256,#6257,#6258,#6259));
#1482=EDGE_LOOP('',(#6260,#6261,#6262,#6263));
#1483=EDGE_LOOP('',(#6264,#6265,#6266,#6267));
#1484=EDGE_LOOP('',(#6268,#6269,#6270,#6271));
#1485=EDGE_LOOP('',(#6272,#6273,#6274,#6275,#6276));
#1486=EDGE_LOOP('',(#6277,#6278,#6279,#6280,#6281,#6282,#6283,#6284,#6285,
#6286));
#1487=EDGE_LOOP('',(#6287,#6288,#6289,#6290,#6291));
#1488=EDGE_LOOP('',(#6292,#6293,#6294,#6295));
#1489=EDGE_LOOP('',(#6296,#6297,#6298,#6299));
#1490=EDGE_LOOP('',(#6300,#6301,#6302,#6303));
#1491=EDGE_LOOP('',(#6304,#6305,#6306,#6307));
#1492=EDGE_LOOP('',(#6308,#6309,#6310,#6311));
#1493=EDGE_LOOP('',(#6312,#6313,#6314,#6315));
#1494=EDGE_LOOP('',(#6316,#6317,#6318,#6319,#6320,#6321,#6322,#6323,#6324,
#6325));
#1495=EDGE_LOOP('',(#6326,#6327,#6328,#6329,#6330,#6331,#6332));
#1496=EDGE_LOOP('',(#6333,#6334,#6335,#6336));
#1497=EDGE_LOOP('',(#6337,#6338,#6339,#6340));
#1498=EDGE_LOOP('',(#6341,#6342,#6343,#6344));
#1499=EDGE_LOOP('',(#6345,#6346,#6347,#6348));
#1500=EDGE_LOOP('',(#6349,#6350,#6351,#6352));
#1501=EDGE_LOOP('',(#6353,#6354,#6355,#6356));
#1502=EDGE_LOOP('',(#6357,#6358,#6359,#6360));
#1503=EDGE_LOOP('',(#6361,#6362,#6363,#6364));
#1504=EDGE_LOOP('',(#6365,#6366,#6367,#6368));
#1505=EDGE_LOOP('',(#6369,#6370,#6371,#6372));
#1506=EDGE_LOOP('',(#6373,#6374,#6375,#6376));
#1507=EDGE_LOOP('',(#6377,#6378,#6379,#6380));
#1508=EDGE_LOOP('',(#6381,#6382,#6383,#6384));
#1509=EDGE_LOOP('',(#6385,#6386,#6387,#6388));
#1510=EDGE_LOOP('',(#6389,#6390,#6391,#6392));
#1511=EDGE_LOOP('',(#6393,#6394,#6395,#6396,#6397,#6398,#6399,#6400,#6401,
#6402));
#1512=EDGE_LOOP('',(#6403,#6404,#6405,#6406));
#1513=EDGE_LOOP('',(#6407,#6408,#6409,#6410));
#1514=EDGE_LOOP('',(#6411,#6412,#6413,#6414));
#1515=EDGE_LOOP('',(#6415,#6416,#6417,#6418));
#1516=EDGE_LOOP('',(#6419,#6420,#6421,#6422));
#1517=EDGE_LOOP('',(#6423,#6424,#6425,#6426));
#1518=EDGE_LOOP('',(#6427,#6428,#6429,#6430));
#1519=EDGE_LOOP('',(#6431,#6432,#6433,#6434));
#1520=EDGE_LOOP('',(#6435,#6436,#6437,#6438));
#1521=EDGE_LOOP('',(#6439,#6440,#6441,#6442));
#1522=EDGE_LOOP('',(#6443,#6444,#6445,#6446,#6447,#6448,#6449,#6450,#6451,
#6452));
#1523=EDGE_LOOP('',(#6453,#6454,#6455,#6456));
#1524=EDGE_LOOP('',(#6457,#6458,#6459,#6460));
#1525=EDGE_LOOP('',(#6461,#6462,#6463,#6464));
#1526=EDGE_LOOP('',(#6465,#6466,#6467,#6468));
#1527=EDGE_LOOP('',(#6469,#6470,#6471,#6472));
#1528=EDGE_LOOP('',(#6473,#6474,#6475,#6476));
#1529=EDGE_LOOP('',(#6477,#6478,#6479,#6480));
#1530=EDGE_LOOP('',(#6481,#6482,#6483,#6484));
#1531=EDGE_LOOP('',(#6485,#6486,#6487,#6488));
#1532=EDGE_LOOP('',(#6489,#6490,#6491,#6492));
#1533=EDGE_LOOP('',(#6493,#6494,#6495,#6496));
#1534=EDGE_LOOP('',(#6497,#6498,#6499,#6500,#6501,#6502,#6503,#6504,#6505,
#6506,#6507));
#1535=EDGE_LOOP('',(#6508,#6509,#6510,#6511));
#1536=EDGE_LOOP('',(#6512,#6513,#6514,#6515));
#1537=EDGE_LOOP('',(#6516,#6517,#6518,#6519));
#1538=EDGE_LOOP('',(#6520,#6521,#6522,#6523));
#1539=EDGE_LOOP('',(#6524,#6525,#6526,#6527));
#1540=EDGE_LOOP('',(#6528,#6529,#6530,#6531));
#1541=EDGE_LOOP('',(#6532,#6533,#6534,#6535));
#1542=EDGE_LOOP('',(#6536,#6537,#6538,#6539));
#1543=EDGE_LOOP('',(#6540,#6541,#6542,#6543));
#1544=EDGE_LOOP('',(#6544,#6545,#6546,#6547));
#1545=EDGE_LOOP('',(#6548,#6549,#6550,#6551,#6552,#6553,#6554,#6555,#6556,
#6557));
#1546=EDGE_LOOP('',(#6558,#6559,#6560,#6561));
#1547=EDGE_LOOP('',(#6562,#6563,#6564,#6565));
#1548=EDGE_LOOP('',(#6566,#6567,#6568,#6569));
#1549=EDGE_LOOP('',(#6570,#6571,#6572,#6573));
#1550=EDGE_LOOP('',(#6574,#6575,#6576,#6577));
#1551=EDGE_LOOP('',(#6578,#6579,#6580,#6581));
#1552=EDGE_LOOP('',(#6582,#6583,#6584,#6585));
#1553=EDGE_LOOP('',(#6586,#6587,#6588,#6589));
#1554=EDGE_LOOP('',(#6590,#6591,#6592,#6593));
#1555=EDGE_LOOP('',(#6594,#6595,#6596,#6597));
#1556=EDGE_LOOP('',(#6598,#6599,#6600,#6601));
#1557=EDGE_LOOP('',(#6602,#6603,#6604,#6605,#6606,#6607,#6608,#6609,#6610,
#6611,#6612));
#1558=EDGE_LOOP('',(#6613,#6614,#6615,#6616));
#1559=EDGE_LOOP('',(#6617,#6618,#6619,#6620));
#1560=EDGE_LOOP('',(#6621,#6622,#6623,#6624));
#1561=EDGE_LOOP('',(#6625,#6626,#6627,#6628));
#1562=EDGE_LOOP('',(#6629,#6630,#6631,#6632));
#1563=EDGE_LOOP('',(#6633,#6634,#6635,#6636));
#1564=EDGE_LOOP('',(#6637,#6638,#6639,#6640));
#1565=EDGE_LOOP('',(#6641,#6642,#6643,#6644));
#1566=EDGE_LOOP('',(#6645,#6646,#6647,#6648));
#1567=EDGE_LOOP('',(#6649,#6650,#6651,#6652));
#1568=EDGE_LOOP('',(#6653,#6654,#6655,#6656,#6657,#6658,#6659,#6660,#6661,
#6662));
#1569=EDGE_LOOP('',(#6663,#6664,#6665,#6666));
#1570=EDGE_LOOP('',(#6667,#6668,#6669,#6670));
#1571=EDGE_LOOP('',(#6671,#6672,#6673,#6674));
#1572=EDGE_LOOP('',(#6675,#6676,#6677,#6678));
#1573=EDGE_LOOP('',(#6679,#6680,#6681,#6682));
#1574=EDGE_LOOP('',(#6683,#6684,#6685,#6686));
#1575=EDGE_LOOP('',(#6687,#6688,#6689,#6690));
#1576=EDGE_LOOP('',(#6691,#6692,#6693,#6694));
#1577=EDGE_LOOP('',(#6695,#6696,#6697,#6698));
#1578=EDGE_LOOP('',(#6699,#6700,#6701,#6702));
#1579=EDGE_LOOP('',(#6703,#6704,#6705,#6706));
#1580=EDGE_LOOP('',(#6707,#6708,#6709,#6710,#6711,#6712,#6713,#6714,#6715,
#6716,#6717));
#1581=EDGE_LOOP('',(#6718,#6719,#6720,#6721));
#1582=EDGE_LOOP('',(#6722,#6723,#6724,#6725));
#1583=EDGE_LOOP('',(#6726,#6727,#6728,#6729));
#1584=EDGE_LOOP('',(#6730,#6731,#6732,#6733));
#1585=EDGE_LOOP('',(#6734,#6735,#6736,#6737));
#1586=EDGE_LOOP('',(#6738,#6739,#6740,#6741));
#1587=EDGE_LOOP('',(#6742,#6743,#6744,#6745));
#1588=EDGE_LOOP('',(#6746,#6747,#6748,#6749));
#1589=EDGE_LOOP('',(#6750,#6751,#6752,#6753));
#1590=EDGE_LOOP('',(#6754,#6755,#6756,#6757));
#1591=EDGE_LOOP('',(#6758,#6759,#6760,#6761));
#1592=EDGE_LOOP('',(#6762,#6763,#6764,#6765));
#1593=EDGE_LOOP('',(#6766,#6767,#6768,#6769));
#1594=EDGE_LOOP('',(#6770,#6771,#6772,#6773));
#1595=EDGE_LOOP('',(#6774,#6775,#6776,#6777));
#1596=EDGE_LOOP('',(#6778,#6779,#6780,#6781));
#1597=EDGE_LOOP('',(#6782,#6783,#6784,#6785));
#1598=EDGE_LOOP('',(#6786,#6787,#6788,#6789));
#1599=EDGE_LOOP('',(#6790,#6791,#6792,#6793));
#1600=EDGE_LOOP('',(#6794,#6795,#6796,#6797));
#1601=EDGE_LOOP('',(#6798,#6799,#6800,#6801,#6802,#6803,#6804,#6805));
#1602=EDGE_LOOP('',(#6806));
#1603=EDGE_LOOP('',(#6807));
#1604=EDGE_LOOP('',(#6808));
#1605=EDGE_LOOP('',(#6809));
#1606=EDGE_LOOP('',(#6810));
#1607=EDGE_LOOP('',(#6811,#6812,#6813,#6814));
#1608=EDGE_LOOP('',(#6815,#6816,#6817,#6818,#6819,#6820,#6821,#6822));
#1609=EDGE_LOOP('',(#6823));
#1610=EDGE_LOOP('',(#6824));
#1611=EDGE_LOOP('',(#6825));
#1612=EDGE_LOOP('',(#6826));
#1613=EDGE_LOOP('',(#6827));
#1614=EDGE_LOOP('',(#6828,#6829,#6830,#6831));
#1615=EDGE_LOOP('',(#6832,#6833,#6834,#6835));
#1616=EDGE_LOOP('',(#6836,#6837,#6838,#6839));
#1617=EDGE_LOOP('',(#6840,#6841,#6842,#6843));
#1618=EDGE_LOOP('',(#6844,#6845,#6846,#6847));
#1619=EDGE_LOOP('',(#6848,#6849,#6850,#6851));
#1620=EDGE_LOOP('',(#6852,#6853,#6854,#6855));
#1621=EDGE_LOOP('',(#6856,#6857,#6858,#6859));
#1622=EDGE_LOOP('',(#6860,#6861,#6862,#6863));
#1623=EDGE_LOOP('',(#6864,#6865,#6866,#6867));
#1624=EDGE_LOOP('',(#6868,#6869,#6870,#6871));
#1625=EDGE_LOOP('',(#6872,#6873,#6874,#6875));
#1626=EDGE_LOOP('',(#6876,#6877,#6878,#6879));
#1627=EDGE_LOOP('',(#6880,#6881,#6882,#6883));
#1628=EDGE_LOOP('',(#6884,#6885,#6886,#6887));
#1629=EDGE_LOOP('',(#6888,#6889,#6890,#6891));
#1630=EDGE_LOOP('',(#6892,#6893,#6894,#6895));
#1631=EDGE_LOOP('',(#6896,#6897,#6898,#6899));
#1632=EDGE_LOOP('',(#6900,#6901,#6902,#6903));
#1633=EDGE_LOOP('',(#6904,#6905,#6906,#6907));
#1634=EDGE_LOOP('',(#6908,#6909,#6910,#6911));
#1635=EDGE_LOOP('',(#6912,#6913,#6914,#6915));
#1636=EDGE_LOOP('',(#6916,#6917,#6918,#6919));
#1637=EDGE_LOOP('',(#6920,#6921,#6922,#6923));
#1638=EDGE_LOOP('',(#6924,#6925,#6926,#6927));
#1639=EDGE_LOOP('',(#6928,#6929,#6930,#6931,#6932,#6933,#6934,#6935,#6936,
#6937,#6938,#6939,#6940,#6941,#6942,#6943,#6944,#6945,#6946,#6947,#6948,
#6949,#6950,#6951));
#1640=EDGE_LOOP('',(#6952));
#1641=EDGE_LOOP('',(#6953));
#1642=EDGE_LOOP('',(#6954,#6955,#6956,#6957));
#1643=EDGE_LOOP('',(#6958,#6959,#6960,#6961));
#1644=EDGE_LOOP('',(#6962,#6963,#6964,#6965));
#1645=EDGE_LOOP('',(#6966,#6967,#6968,#6969,#6970,#6971));
#1646=EDGE_LOOP('',(#6972,#6973,#6974,#6975));
#1647=EDGE_LOOP('',(#6976,#6977,#6978,#6979,#6980,#6981));
#1648=EDGE_LOOP('',(#6982,#6983,#6984,#6985,#6986));
#1649=EDGE_LOOP('',(#6987,#6988,#6989,#6990,#6991,#6992));
#1650=EDGE_LOOP('',(#6993,#6994,#6995,#6996,#6997,#6998));
#1651=EDGE_LOOP('',(#6999,#7000,#7001,#7002,#7003));
#1652=EDGE_LOOP('',(#7004,#7005,#7006,#7007));
#1653=EDGE_LOOP('',(#7008,#7009,#7010,#7011,#7012,#7013,#7014,#7015,#7016,
#7017,#7018,#7019,#7020,#7021,#7022,#7023,#7024,#7025,#7026,#7027,#7028,
#7029,#7030,#7031));
#1654=EDGE_LOOP('',(#7032));
#1655=EDGE_LOOP('',(#7033));
#1656=EDGE_LOOP('',(#7034,#7035,#7036,#7037));
#1657=EDGE_LOOP('',(#7038,#7039,#7040,#7041));
#1658=EDGE_LOOP('',(#7042,#7043,#7044,#7045));
#1659=EDGE_LOOP('',(#7046,#7047,#7048));
#1660=EDGE_LOOP('',(#7049,#7050,#7051,#7052,#7053));
#1661=EDGE_LOOP('',(#7054,#7055,#7056,#7057));
#1662=EDGE_LOOP('',(#7058,#7059,#7060));
#1663=EDGE_LOOP('',(#7061,#7062,#7063,#7064));
#1664=EDGE_LOOP('',(#7065,#7066,#7067,#7068));
#1665=EDGE_LOOP('',(#7069,#7070,#7071,#7072));
#1666=EDGE_LOOP('',(#7073,#7074,#7075));
#1667=EDGE_LOOP('',(#7076,#7077,#7078,#7079,#7080));
#1668=EDGE_LOOP('',(#7081,#7082,#7083));
#1669=EDGE_LOOP('',(#7084,#7085,#7086,#7087));
#1670=EDGE_LOOP('',(#7088,#7089,#7090,#7091,#7092));
#1671=EDGE_LOOP('',(#7093,#7094,#7095,#7096));
#1672=EDGE_LOOP('',(#7097,#7098,#7099,#7100));
#1673=EDGE_LOOP('',(#7101,#7102,#7103,#7104));
#1674=EDGE_LOOP('',(#7105));
#1675=EDGE_LOOP('',(#7106));
#1676=EDGE_LOOP('',(#7107));
#1677=EDGE_LOOP('',(#7108,#7109,#7110,#7111,#7112,#7113,#7114,#7115));
#1678=EDGE_LOOP('',(#7116,#7117,#7118,#7119));
#1679=EDGE_LOOP('',(#7120,#7121,#7122,#7123));
#1680=EDGE_LOOP('',(#7124,#7125,#7126,#7127,#7128));
#1681=EDGE_LOOP('',(#7129,#7130,#7131,#7132));
#1682=EDGE_LOOP('',(#7133,#7134,#7135,#7136));
#1683=EDGE_LOOP('',(#7137,#7138,#7139,#7140));
#1684=EDGE_LOOP('',(#7141,#7142,#7143,#7144));
#1685=EDGE_LOOP('',(#7145,#7146,#7147,#7148));
#1686=EDGE_LOOP('',(#7149,#7150,#7151,#7152));
#1687=EDGE_LOOP('',(#7153,#7154,#7155,#7156));
#1688=EDGE_LOOP('',(#7157,#7158,#7159,#7160));
#1689=EDGE_LOOP('',(#7161,#7162,#7163,#7164));
#1690=EDGE_LOOP('',(#7165,#7166,#7167,#7168));
#1691=EDGE_LOOP('',(#7169,#7170,#7171,#7172));
#1692=EDGE_LOOP('',(#7173,#7174,#7175,#7176));
#1693=EDGE_LOOP('',(#7177,#7178,#7179,#7180));
#1694=EDGE_LOOP('',(#7181,#7182,#7183,#7184));
#1695=EDGE_LOOP('',(#7185,#7186,#7187,#7188));
#1696=EDGE_LOOP('',(#7189,#7190,#7191,#7192));
#1697=EDGE_LOOP('',(#7193,#7194,#7195,#7196));
#1698=EDGE_LOOP('',(#7197,#7198,#7199,#7200));
#1699=EDGE_LOOP('',(#7201,#7202,#7203,#7204));
#1700=EDGE_LOOP('',(#7205,#7206,#7207,#7208));
#1701=EDGE_LOOP('',(#7209,#7210,#7211,#7212));
#1702=EDGE_LOOP('',(#7213,#7214,#7215,#7216,#7217,#7218));
#1703=EDGE_LOOP('',(#7219,#7220,#7221,#7222));
#1704=EDGE_LOOP('',(#7223,#7224,#7225,#7226));
#1705=EDGE_LOOP('',(#7227,#7228,#7229,#7230));
#1706=EDGE_LOOP('',(#7231,#7232,#7233,#7234));
#1707=EDGE_LOOP('',(#7235,#7236,#7237,#7238));
#1708=EDGE_LOOP('',(#7239,#7240,#7241,#7242));
#1709=EDGE_LOOP('',(#7243,#7244,#7245,#7246));
#1710=EDGE_LOOP('',(#7247,#7248,#7249,#7250));
#1711=EDGE_LOOP('',(#7251,#7252,#7253,#7254));
#1712=EDGE_LOOP('',(#7255,#7256,#7257,#7258));
#1713=EDGE_LOOP('',(#7259,#7260,#7261,#7262));
#1714=EDGE_LOOP('',(#7263,#7264,#7265,#7266));
#1715=EDGE_LOOP('',(#7267,#7268,#7269,#7270));
#1716=EDGE_LOOP('',(#7271,#7272,#7273,#7274));
#1717=EDGE_LOOP('',(#7275,#7276,#7277,#7278));
#1718=EDGE_LOOP('',(#7279,#7280,#7281,#7282));
#1719=EDGE_LOOP('',(#7283,#7284,#7285,#7286));
#1720=EDGE_LOOP('',(#7287,#7288,#7289,#7290));
#1721=EDGE_LOOP('',(#7291,#7292,#7293,#7294));
#1722=EDGE_LOOP('',(#7295,#7296,#7297,#7298));
#1723=EDGE_LOOP('',(#7299,#7300,#7301,#7302));
#1724=EDGE_LOOP('',(#7303));
#1725=EDGE_LOOP('',(#7304));
#1726=EDGE_LOOP('',(#7305));
#1727=EDGE_LOOP('',(#7306,#7307,#7308,#7309));
#1728=EDGE_LOOP('',(#7310,#7311,#7312,#7313));
#1729=EDGE_LOOP('',(#7314,#7315,#7316,#7317));
#1730=EDGE_LOOP('',(#7318,#7319,#7320,#7321));
#1731=EDGE_LOOP('',(#7322,#7323,#7324,#7325));
#1732=EDGE_LOOP('',(#7326,#7327,#7328,#7329));
#1733=EDGE_LOOP('',(#7330,#7331,#7332,#7333));
#1734=EDGE_LOOP('',(#7334,#7335,#7336,#7337));
#1735=EDGE_LOOP('',(#7338));
#1736=EDGE_LOOP('',(#7339));
#1737=EDGE_LOOP('',(#7340));
#1738=EDGE_LOOP('',(#7341));
#1739=EDGE_LOOP('',(#7342,#7343,#7344,#7345));
#1740=EDGE_LOOP('',(#7346,#7347,#7348,#7349));
#1741=EDGE_LOOP('',(#7350,#7351,#7352,#7353));
#1742=EDGE_LOOP('',(#7354,#7355,#7356,#7357));
#1743=EDGE_LOOP('',(#7358));
#1744=EDGE_LOOP('',(#7359,#7360,#7361,#7362));
#1745=EDGE_LOOP('',(#7363,#7364,#7365,#7366));
#1746=EDGE_LOOP('',(#7367,#7368,#7369,#7370));
#1747=EDGE_LOOP('',(#7371));
#1748=EDGE_LOOP('',(#7372,#7373,#7374,#7375,#7376));
#1749=EDGE_LOOP('',(#7377,#7378,#7379,#7380,#7381));
#1750=EDGE_LOOP('',(#7382));
#1751=EDGE_LOOP('',(#7383,#7384,#7385,#7386));
#1752=EDGE_LOOP('',(#7387,#7388,#7389,#7390,#7391));
#1753=EDGE_LOOP('',(#7392,#7393));
#1754=EDGE_LOOP('',(#7394,#7395));
#1755=EDGE_LOOP('',(#7396,#7397,#7398,#7399));
#1756=EDGE_LOOP('',(#7400,#7401,#7402,#7403,#7404,#7405,#7406,#7407));
#1757=EDGE_LOOP('',(#7408));
#1758=EDGE_LOOP('',(#7409));
#1759=EDGE_LOOP('',(#7410,#7411,#7412,#7413));
#1760=EDGE_LOOP('',(#7414,#7415,#7416,#7417,#7418));
#1761=EDGE_LOOP('',(#7419));
#1762=EDGE_LOOP('',(#7420,#7421,#7422,#7423,#7424));
#1763=EDGE_LOOP('',(#7425,#7426,#7427,#7428));
#1764=EDGE_LOOP('',(#7429));
#1765=EDGE_LOOP('',(#7430));
#1766=EDGE_LOOP('',(#7431,#7432,#7433,#7434));
#1767=EDGE_LOOP('',(#7435,#7436,#7437,#7438));
#1768=EDGE_LOOP('',(#7439));
#1769=EDGE_LOOP('',(#7440,#7441,#7442,#7443,#7444));
#1770=EDGE_LOOP('',(#7445));
#1771=EDGE_LOOP('',(#7446));
#1772=EDGE_LOOP('',(#7447,#7448,#7449,#7450,#7451));
#1773=EDGE_LOOP('',(#7452,#7453,#7454,#7455));
#1774=EDGE_LOOP('',(#7456));
#1775=EDGE_LOOP('',(#7457));
#1776=EDGE_LOOP('',(#7458,#7459,#7460,#7461));
#1777=EDGE_LOOP('',(#7462));
#1778=EDGE_LOOP('',(#7463));
#1779=EDGE_LOOP('',(#7464,#7465,#7466,#7467));
#1780=EDGE_LOOP('',(#7468,#7469,#7470,#7471));
#1781=EDGE_LOOP('',(#7472,#7473,#7474,#7475,#7476,#7477));
#1782=EDGE_LOOP('',(#7478,#7479,#7480,#7481));
#1783=EDGE_LOOP('',(#7482,#7483,#7484,#7485));
#1784=EDGE_LOOP('',(#7486,#7487,#7488,#7489));
#1785=EDGE_LOOP('',(#7490,#7491,#7492,#7493));
#1786=EDGE_LOOP('',(#7494,#7495,#7496,#7497,#7498,#7499));
#1787=EDGE_LOOP('',(#7500,#7501,#7502,#7503));
#1788=EDGE_LOOP('',(#7504,#7505,#7506,#7507));
#1789=EDGE_LOOP('',(#7508,#7509,#7510,#7511));
#1790=EDGE_LOOP('',(#7512,#7513,#7514,#7515,#7516));
#1791=EDGE_LOOP('',(#7517,#7518,#7519,#7520,#7521,#7522,#7523,#7524,#7525,
#7526,#7527,#7528,#7529,#7530,#7531,#7532));
#1792=EDGE_LOOP('',(#7533));
#1793=EDGE_LOOP('',(#7534));
#1794=EDGE_LOOP('',(#7535,#7536,#7537,#7538));
#1795=EDGE_LOOP('',(#7539,#7540,#7541,#7542));
#1796=EDGE_LOOP('',(#7543,#7544,#7545,#7546));
#1797=EDGE_LOOP('',(#7547,#7548,#7549,#7550));
#1798=EDGE_LOOP('',(#7551,#7552,#7553,#7554));
#1799=EDGE_LOOP('',(#7555,#7556,#7557,#7558));
#1800=EDGE_LOOP('',(#7559,#7560,#7561,#7562));
#1801=EDGE_LOOP('',(#7563,#7564,#7565,#7566));
#1802=EDGE_LOOP('',(#7567,#7568,#7569,#7570));
#1803=EDGE_LOOP('',(#7571,#7572,#7573,#7574));
#1804=EDGE_LOOP('',(#7575,#7576,#7577,#7578));
#1805=EDGE_LOOP('',(#7579,#7580,#7581,#7582));
#1806=EDGE_LOOP('',(#7583,#7584,#7585,#7586));
#1807=EDGE_LOOP('',(#7587,#7588,#7589,#7590));
#1808=EDGE_LOOP('',(#7591,#7592,#7593,#7594));
#1809=EDGE_LOOP('',(#7595,#7596,#7597,#7598));
#1810=EDGE_LOOP('',(#7599,#7600,#7601,#7602));
#1811=EDGE_LOOP('',(#7603,#7604,#7605,#7606));
#1812=EDGE_LOOP('',(#7607,#7608,#7609,#7610));
#1813=EDGE_LOOP('',(#7611,#7612,#7613,#7614));
#1814=EDGE_LOOP('',(#7615,#7616,#7617,#7618));
#1815=EDGE_LOOP('',(#7619,#7620,#7621,#7622));
#1816=EDGE_LOOP('',(#7623,#7624,#7625,#7626));
#1817=EDGE_LOOP('',(#7627,#7628,#7629,#7630));
#1818=EDGE_LOOP('',(#7631,#7632,#7633,#7634));
#1819=EDGE_LOOP('',(#7635,#7636,#7637,#7638));
#1820=EDGE_LOOP('',(#7639,#7640,#7641,#7642,#7643,#7644,#7645,#7646,#7647,
#7648,#7649,#7650));
#1821=EDGE_LOOP('',(#7651,#7652,#7653,#7654,#7655,#7656,#7657,#7658,#7659,
#7660,#7661,#7662,#7663,#7664,#7665,#7666,#7667,#7668,#7669,#7670,#7671,
#7672,#7673,#7674,#7675));
#1822=EDGE_LOOP('',(#7676,#7677,#7678,#7679));
#1823=EDGE_LOOP('',(#7680,#7681,#7682,#7683,#7684,#7685));
#1824=EDGE_LOOP('',(#7686,#7687,#7688,#7689));
#1825=EDGE_LOOP('',(#7690,#7691,#7692,#7693));
#1826=EDGE_LOOP('',(#7694,#7695,#7696,#7697));
#1827=EDGE_LOOP('',(#7698,#7699,#7700,#7701));
#1828=EDGE_LOOP('',(#7702,#7703,#7704,#7705,#7706,#7707));
#1829=EDGE_LOOP('',(#7708,#7709,#7710,#7711));
#1830=EDGE_LOOP('',(#7712,#7713,#7714,#7715));
#1831=EDGE_LOOP('',(#7716,#7717,#7718,#7719));
#1832=EDGE_LOOP('',(#7720,#7721,#7722,#7723));
#1833=EDGE_LOOP('',(#7724,#7725,#7726,#7727,#7728,#7729,#7730,#7731,#7732,
#7733,#7734,#7735));
#1834=EDGE_LOOP('',(#7736,#7737,#7738,#7739));
#1835=EDGE_LOOP('',(#7740,#7741,#7742,#7743,#7744,#7745));
#1836=EDGE_LOOP('',(#7746,#7747,#7748,#7749));
#1837=EDGE_LOOP('',(#7750,#7751,#7752,#7753,#7754,#7755));
#1838=EDGE_LOOP('',(#7756,#7757,#7758,#7759));
#1839=EDGE_LOOP('',(#7760,#7761,#7762,#7763));
#1840=EDGE_LOOP('',(#7764,#7765,#7766,#7767));
#1841=EDGE_LOOP('',(#7768,#7769,#7770,#7771));
#1842=EDGE_LOOP('',(#7772,#7773,#7774,#7775));
#1843=EDGE_LOOP('',(#7776,#7777,#7778,#7779));
#1844=EDGE_LOOP('',(#7780,#7781,#7782,#7783,#7784,#7785,#7786,#7787,#7788,
#7789,#7790,#7791));
#1845=EDGE_LOOP('',(#7792,#7793,#7794,#7795));
#1846=EDGE_LOOP('',(#7796,#7797,#7798,#7799));
#1847=EDGE_LOOP('',(#7800,#7801,#7802,#7803,#7804,#7805,#7806,#7807,#7808,
#7809,#7810,#7811));
#1848=EDGE_LOOP('',(#7812,#7813,#7814,#7815,#7816,#7817,#7818,#7819,#7820,
#7821,#7822,#7823,#7824,#7825,#7826,#7827,#7828,#7829,#7830,#7831,#7832,
#7833,#7834,#7835,#7836));
#1849=EDGE_LOOP('',(#7837,#7838,#7839,#7840));
#1850=EDGE_LOOP('',(#7841,#7842,#7843,#7844));
#1851=EDGE_LOOP('',(#7845,#7846,#7847,#7848));
#1852=EDGE_LOOP('',(#7849,#7850,#7851));
#1853=EDGE_LOOP('',(#7852,#7853));
#1854=EDGE_LOOP('',(#7854,#7855,#7856,#7857));
#1855=EDGE_LOOP('',(#7858,#7859));
#1856=EDGE_LOOP('',(#7860));
#1857=EDGE_LOOP('',(#7861));
#1858=EDGE_LOOP('',(#7862,#7863,#7864,#7865));
#1859=EDGE_LOOP('',(#7866,#7867,#7868,#7869));
#1860=EDGE_LOOP('',(#7870,#7871,#7872,#7873));
#1861=EDGE_LOOP('',(#7874,#7875,#7876,#7877));
#1862=EDGE_LOOP('',(#7878,#7879,#7880,#7881));
#1863=EDGE_LOOP('',(#7882,#7883,#7884,#7885));
#1864=EDGE_LOOP('',(#7886,#7887,#7888));
#1865=EDGE_LOOP('',(#7889,#7890,#7891,#7892,#7893));
#1866=EDGE_LOOP('',(#7894,#7895,#7896,#7897));
#1867=EDGE_LOOP('',(#7898,#7899,#7900,#7901));
#1868=EDGE_LOOP('',(#7902,#7903,#7904,#7905));
#1869=EDGE_LOOP('',(#7906,#7907,#7908,#7909,#7910,#7911));
#1870=EDGE_LOOP('',(#7912,#7913,#7914,#7915,#7916,#7917,#7918,#7919,#7920,
#7921,#7922,#7923,#7924));
#1871=EDGE_LOOP('',(#7925,#7926,#7927,#7928,#7929));
#1872=EDGE_LOOP('',(#7930,#7931,#7932,#7933));
#1873=EDGE_LOOP('',(#7934,#7935,#7936,#7937,#7938,#7939,#7940,#7941,#7942,
#7943,#7944,#7945,#7946,#7947));
#1874=EDGE_LOOP('',(#7948,#7949,#7950,#7951));
#1875=EDGE_LOOP('',(#7952,#7953,#7954,#7955));
#1876=EDGE_LOOP('',(#7956,#7957,#7958,#7959));
#1877=EDGE_LOOP('',(#7960,#7961,#7962,#7963));
#1878=EDGE_LOOP('',(#7964,#7965,#7966,#7967));
#1879=EDGE_LOOP('',(#7968,#7969,#7970,#7971));
#1880=EDGE_LOOP('',(#7972,#7973,#7974,#7975,#7976,#7977));
#1881=EDGE_LOOP('',(#7978));
#1882=EDGE_LOOP('',(#7979,#7980,#7981,#7982,#7983,#7984));
#1883=EDGE_LOOP('',(#7985,#7986,#7987,#7988));
#1884=EDGE_LOOP('',(#7989,#7990,#7991,#7992,#7993,#7994));
#1885=EDGE_LOOP('',(#7995));
#1886=EDGE_LOOP('',(#7996,#7997,#7998,#7999,#8000,#8001));
#1887=EDGE_LOOP('',(#8002,#8003,#8004,#8005));
#1888=EDGE_LOOP('',(#8006,#8007,#8008,#8009));
#1889=EDGE_LOOP('',(#8010,#8011,#8012,#8013));
#1890=EDGE_LOOP('',(#8014,#8015,#8016,#8017));
#1891=EDGE_LOOP('',(#8018,#8019,#8020,#8021));
#1892=EDGE_LOOP('',(#8022,#8023,#8024,#8025));
#1893=EDGE_LOOP('',(#8026,#8027,#8028,#8029));
#1894=EDGE_LOOP('',(#8030,#8031,#8032,#8033));
#1895=EDGE_LOOP('',(#8034,#8035,#8036,#8037));
#1896=EDGE_LOOP('',(#8038,#8039,#8040,#8041));
#1897=EDGE_LOOP('',(#8042,#8043,#8044,#8045));
#1898=EDGE_LOOP('',(#8046,#8047,#8048,#8049));
#1899=EDGE_LOOP('',(#8050,#8051,#8052,#8053));
#1900=EDGE_LOOP('',(#8054,#8055,#8056,#8057));
#1901=EDGE_LOOP('',(#8058,#8059,#8060,#8061));
#1902=EDGE_LOOP('',(#8062,#8063,#8064,#8065));
#1903=EDGE_LOOP('',(#8066,#8067,#8068,#8069));
#1904=EDGE_LOOP('',(#8070,#8071,#8072,#8073));
#1905=EDGE_LOOP('',(#8074,#8075,#8076,#8077));
#1906=EDGE_LOOP('',(#8078,#8079,#8080,#8081));
#1907=EDGE_LOOP('',(#8082,#8083,#8084,#8085));
#1908=EDGE_LOOP('',(#8086,#8087,#8088,#8089));
#1909=EDGE_LOOP('',(#8090,#8091,#8092,#8093));
#1910=EDGE_LOOP('',(#8094,#8095,#8096,#8097));
#1911=EDGE_LOOP('',(#8098,#8099,#8100,#8101,#8102));
#1912=EDGE_LOOP('',(#8103,#8104,#8105,#8106,#8107,#8108,#8109,#8110,#8111,
#8112,#8113,#8114,#8115,#8116,#8117,#8118,#8119,#8120,#8121,#8122,#8123,
#8124,#8125,#8126,#8127,#8128,#8129,#8130));
#1913=EDGE_LOOP('',(#8131,#8132,#8133,#8134,#8135));
#1914=EDGE_LOOP('',(#8136,#8137,#8138,#8139));
#1915=EDGE_LOOP('',(#8140,#8141,#8142,#8143,#8144,#8145,#8146,#8147,#8148,
#8149,#8150,#8151,#8152,#8153,#8154,#8155,#8156,#8157,#8158,#8159,#8160,
#8161,#8162,#8163,#8164,#8165,#8166,#8167));
#1916=EDGE_LOOP('',(#8168,#8169,#8170));
#1917=EDGE_LOOP('',(#8171,#8172,#8173,#8174));
#1918=EDGE_LOOP('',(#8175,#8176,#8177,#8178));
#1919=EDGE_LOOP('',(#8179,#8180,#8181,#8182));
#1920=EDGE_LOOP('',(#8183,#8184,#8185,#8186));
#1921=EDGE_LOOP('',(#8187,#8188,#8189,#8190));
#1922=EDGE_LOOP('',(#8191,#8192,#8193,#8194));
#1923=EDGE_LOOP('',(#8195,#8196,#8197,#8198,#8199,#8200));
#1924=EDGE_LOOP('',(#8201));
#1925=EDGE_LOOP('',(#8202));
#1926=EDGE_LOOP('',(#8203,#8204,#8205,#8206,#8207,#8208));
#1927=EDGE_LOOP('',(#8209,#8210,#8211,#8212));
#1928=EDGE_LOOP('',(#8213,#8214,#8215,#8216,#8217,#8218));
#1929=EDGE_LOOP('',(#8219));
#1930=EDGE_LOOP('',(#8220,#8221,#8222,#8223,#8224,#8225));
#1931=EDGE_LOOP('',(#8226));
#1932=EDGE_LOOP('',(#8227,#8228,#8229,#8230));
#1933=EDGE_LOOP('',(#8231,#8232,#8233,#8234));
#1934=EDGE_LOOP('',(#8235,#8236,#8237,#8238));
#1935=EDGE_LOOP('',(#8239));
#1936=LINE('',#12276,#2781);
#1937=LINE('',#12278,#2782);
#1938=LINE('',#12279,#2783);
#1939=LINE('',#12283,#2784);
#1940=LINE('',#12285,#2785);
#1941=LINE('',#12286,#2786);
#1942=LINE('',#12290,#2787);
#1943=LINE('',#12292,#2788);
#1944=LINE('',#12293,#2789);
#1945=LINE('',#12297,#2790);
#1946=LINE('',#12299,#2791);
#1947=LINE('',#12300,#2792);
#1948=LINE('',#12305,#2793);
#1949=LINE('',#12306,#2794);
#1950=LINE('',#12308,#2795);
#1951=LINE('',#12309,#2796);
#1952=LINE('',#12311,#2797);
#1953=LINE('',#12312,#2798);
#1954=LINE('',#12314,#2799);
#1955=LINE('',#12315,#2800);
#1956=LINE('',#12320,#2801);
#1957=LINE('',#12321,#2802);
#1958=LINE('',#12326,#2803);
#1959=LINE('',#12327,#2804);
#1960=LINE('',#12329,#2805);
#1961=LINE('',#12330,#2806);
#1962=LINE('',#12335,#2807);
#1963=LINE('',#12336,#2808);
#1964=LINE('',#12338,#2809);
#1965=LINE('',#12351,#2810);
#1966=LINE('',#12355,#2811);
#1967=LINE('',#12359,#2812);
#1968=LINE('',#12361,#2813);
#1969=LINE('',#12369,#2814);
#1970=LINE('',#12371,#2815);
#1971=LINE('',#12372,#2816);
#1972=LINE('',#12376,#2817);
#1973=LINE('',#12378,#2818);
#1974=LINE('',#12379,#2819);
#1975=LINE('',#12384,#2820);
#1976=LINE('',#12385,#2821);
#1977=LINE('',#12387,#2822);
#1978=LINE('',#12388,#2823);
#1979=LINE('',#12392,#2824);
#1980=LINE('',#12394,#2825);
#1981=LINE('',#12395,#2826);
#1982=LINE('',#12399,#2827);
#1983=LINE('',#12401,#2828);
#1984=LINE('',#12402,#2829);
#1985=LINE('',#12407,#2830);
#1986=LINE('',#12408,#2831);
#1987=LINE('',#12410,#2832);
#1988=LINE('',#12411,#2833);
#1989=LINE('',#12413,#2834);
#1990=LINE('',#12414,#2835);
#1991=LINE('',#12416,#2836);
#1992=LINE('',#12417,#2837);
#1993=LINE('',#12422,#2838);
#1994=LINE('',#12423,#2839);
#1995=LINE('',#12428,#2840);
#1996=LINE('',#12429,#2841);
#1997=LINE('',#12431,#2842);
#1998=LINE('',#12436,#2843);
#1999=LINE('',#12444,#2844);
#2000=LINE('',#12446,#2845);
#2001=LINE('',#12448,#2846);
#2002=LINE('',#12449,#2847);
#2003=LINE('',#12454,#2848);
#2004=LINE('',#12459,#2849);
#2005=LINE('',#12460,#2850);
#2006=LINE('',#12461,#2851);
#2007=LINE('',#12466,#2852);
#2008=LINE('',#12471,#2853);
#2009=LINE('',#12472,#2854);
#2010=LINE('',#12473,#2855);
#2011=LINE('',#12478,#2856);
#2012=LINE('',#12483,#2857);
#2013=LINE('',#12484,#2858);
#2014=LINE('',#12485,#2859);
#2015=LINE('',#12491,#2860);
#2016=LINE('',#12494,#2861);
#2017=LINE('',#12497,#2862);
#2018=LINE('',#12498,#2863);
#2019=LINE('',#12501,#2864);
#2020=LINE('',#12505,#2865);
#2021=LINE('',#12506,#2866);
#2022=LINE('',#12520,#2867);
#2023=LINE('',#12522,#2868);
#2024=LINE('',#12524,#2869);
#2025=LINE('',#12525,#2870);
#2026=LINE('',#12528,#2871);
#2027=LINE('',#12532,#2872);
#2028=LINE('',#12533,#2873);
#2029=LINE('',#12536,#2874);
#2030=LINE('',#12540,#2875);
#2031=LINE('',#12541,#2876);
#2032=LINE('',#12545,#2877);
#2033=LINE('',#12555,#2878);
#2034=LINE('',#12557,#2879);
#2035=LINE('',#12559,#2880);
#2036=LINE('',#12561,#2881);
#2037=LINE('',#12567,#2882);
#2038=LINE('',#12572,#2883);
#2039=LINE('',#12575,#2884);
#2040=LINE('',#12578,#2885);
#2041=LINE('',#12581,#2886);
#2042=LINE('',#12582,#2887);
#2043=LINE('',#12585,#2888);
#2044=LINE('',#12589,#2889);
#2045=LINE('',#12591,#2890);
#2046=LINE('',#12593,#2891);
#2047=LINE('',#12595,#2892);
#2048=LINE('',#12597,#2893);
#2049=LINE('',#12599,#2894);
#2050=LINE('',#12601,#2895);
#2051=LINE('',#12603,#2896);
#2052=LINE('',#12605,#2897);
#2053=LINE('',#12607,#2898);
#2054=LINE('',#12637,#2899);
#2055=LINE('',#12662,#2900);
#2056=LINE('',#12686,#2901);
#2057=LINE('',#12691,#2902);
#2058=LINE('',#12715,#2903);
#2059=LINE('',#12718,#2904);
#2060=LINE('',#12721,#2905);
#2061=LINE('',#12723,#2906);
#2062=LINE('',#12725,#2907);
#2063=LINE('',#12726,#2908);
#2064=LINE('',#12729,#2909);
#2065=LINE('',#12735,#2910);
#2066=LINE('',#12759,#2911);
#2067=LINE('',#12760,#2912);
#2068=LINE('',#12763,#2913);
#2069=LINE('',#12768,#2914);
#2070=LINE('',#12771,#2915);
#2071=LINE('',#12777,#2916);
#2072=LINE('',#12804,#2917);
#2073=LINE('',#12805,#2918);
#2074=LINE('',#12806,#2919);
#2075=LINE('',#12809,#2920);
#2076=LINE('',#12811,#2921);
#2077=LINE('',#12836,#2922);
#2078=LINE('',#12838,#2923);
#2079=LINE('',#12840,#2924);
#2080=LINE('',#12842,#2925);
#2081=LINE('',#12844,#2926);
#2082=LINE('',#12846,#2927);
#2083=LINE('',#12848,#2928);
#2084=LINE('',#12850,#2929);
#2085=LINE('',#12852,#2930);
#2086=LINE('',#12854,#2931);
#2087=LINE('',#12856,#2932);
#2088=LINE('',#12858,#2933);
#2089=LINE('',#12860,#2934);
#2090=LINE('',#12862,#2935);
#2091=LINE('',#12863,#2936);
#2092=LINE('',#12866,#2937);
#2093=LINE('',#12868,#2938);
#2094=LINE('',#12870,#2939);
#2095=LINE('',#12872,#2940);
#2096=LINE('',#12874,#2941);
#2097=LINE('',#12876,#2942);
#2098=LINE('',#12878,#2943);
#2099=LINE('',#12880,#2944);
#2100=LINE('',#12882,#2945);
#2101=LINE('',#12883,#2946);
#2102=LINE('',#12886,#2947);
#2103=LINE('',#12888,#2948);
#2104=LINE('',#12890,#2949);
#2105=LINE('',#12892,#2950);
#2106=LINE('',#12894,#2951);
#2107=LINE('',#12896,#2952);
#2108=LINE('',#12898,#2953);
#2109=LINE('',#12900,#2954);
#2110=LINE('',#12902,#2955);
#2111=LINE('',#12903,#2956);
#2112=LINE('',#12950,#2957);
#2113=LINE('',#12952,#2958);
#2114=LINE('',#12954,#2959);
#2115=LINE('',#12956,#2960);
#2116=LINE('',#12958,#2961);
#2117=LINE('',#12960,#2962);
#2118=LINE('',#12962,#2963);
#2119=LINE('',#12964,#2964);
#2120=LINE('',#12966,#2965);
#2121=LINE('',#12967,#2966);
#2122=LINE('',#13060,#2967);
#2123=LINE('',#13062,#2968);
#2124=LINE('',#13064,#2969);
#2125=LINE('',#13066,#2970);
#2126=LINE('',#13068,#2971);
#2127=LINE('',#13070,#2972);
#2128=LINE('',#13072,#2973);
#2129=LINE('',#13074,#2974);
#2130=LINE('',#13076,#2975);
#2131=LINE('',#13077,#2976);
#2132=LINE('',#13080,#2977);
#2133=LINE('',#13086,#2978);
#2134=LINE('',#13106,#2979);
#2135=LINE('',#13109,#2980);
#2136=LINE('',#13111,#2981);
#2137=LINE('',#13113,#2982);
#2138=LINE('',#13114,#2983);
#2139=LINE('',#13117,#2984);
#2140=LINE('',#13118,#2985);
#2141=LINE('',#13121,#2986);
#2142=LINE('',#13122,#2987);
#2143=LINE('',#13125,#2988);
#2144=LINE('',#13128,#2989);
#2145=LINE('',#13129,#2990);
#2146=LINE('',#13133,#2991);
#2147=LINE('',#13135,#2992);
#2148=LINE('',#13137,#2993);
#2149=LINE('',#13141,#2994);
#2150=LINE('',#13142,#2995);
#2151=LINE('',#13145,#2996);
#2152=LINE('',#13146,#2997);
#2153=LINE('',#13173,#2998);
#2154=LINE('',#13174,#2999);
#2155=LINE('',#13177,#3000);
#2156=LINE('',#13178,#3001);
#2157=LINE('',#13181,#3002);
#2158=LINE('',#13182,#3003);
#2159=LINE('',#13185,#3004);
#2160=LINE('',#13186,#3005);
#2161=LINE('',#13189,#3006);
#2162=LINE('',#13190,#3007);
#2163=LINE('',#13193,#3008);
#2164=LINE('',#13194,#3009);
#2165=LINE('',#13196,#3010);
#2166=LINE('',#13200,#3011);
#2167=LINE('',#13201,#3012);
#2168=LINE('',#13204,#3013);
#2169=LINE('',#13205,#3014);
#2170=LINE('',#13208,#3015);
#2171=LINE('',#13209,#3016);
#2172=LINE('',#13212,#3017);
#2173=LINE('',#13213,#3018);
#2174=LINE('',#13216,#3019);
#2175=LINE('',#13217,#3020);
#2176=LINE('',#13220,#3021);
#2177=LINE('',#13221,#3022);
#2178=LINE('',#13223,#3023);
#2179=LINE('',#13239,#3024);
#2180=LINE('',#13246,#3025);
#2181=LINE('',#13253,#3026);
#2182=LINE('',#13260,#3027);
#2183=LINE('',#13267,#3028);
#2184=LINE('',#13276,#3029);
#2185=LINE('',#13278,#3030);
#2186=LINE('',#13279,#3031);
#2187=LINE('',#13282,#3032);
#2188=LINE('',#13283,#3033);
#2189=LINE('',#13286,#3034);
#2190=LINE('',#13287,#3035);
#2191=LINE('',#13290,#3036);
#2192=LINE('',#13291,#3037);
#2193=LINE('',#13294,#3038);
#2194=LINE('',#13295,#3039);
#2195=LINE('',#13298,#3040);
#2196=LINE('',#13299,#3041);
#2197=LINE('',#13302,#3042);
#2198=LINE('',#13303,#3043);
#2199=LINE('',#13306,#3044);
#2200=LINE('',#13307,#3045);
#2201=LINE('',#13310,#3046);
#2202=LINE('',#13311,#3047);
#2203=LINE('',#13313,#3048);
#2204=LINE('',#13317,#3049);
#2205=LINE('',#13319,#3050);
#2206=LINE('',#13320,#3051);
#2207=LINE('',#13323,#3052);
#2208=LINE('',#13324,#3053);
#2209=LINE('',#13327,#3054);
#2210=LINE('',#13328,#3055);
#2211=LINE('',#13331,#3056);
#2212=LINE('',#13332,#3057);
#2213=LINE('',#13335,#3058);
#2214=LINE('',#13336,#3059);
#2215=LINE('',#13339,#3060);
#2216=LINE('',#13340,#3061);
#2217=LINE('',#13343,#3062);
#2218=LINE('',#13344,#3063);
#2219=LINE('',#13347,#3064);
#2220=LINE('',#13348,#3065);
#2221=LINE('',#13351,#3066);
#2222=LINE('',#13352,#3067);
#2223=LINE('',#13354,#3068);
#2224=LINE('',#13363,#3069);
#2225=LINE('',#13368,#3070);
#2226=LINE('',#13376,#3071);
#2227=LINE('',#13387,#3072);
#2228=LINE('',#13398,#3073);
#2229=LINE('',#13409,#3074);
#2230=LINE('',#13420,#3075);
#2231=LINE('',#13431,#3076);
#2232=LINE('',#13442,#3077);
#2233=LINE('',#13453,#3078);
#2234=LINE('',#13464,#3079);
#2235=LINE('',#13480,#3080);
#2236=LINE('',#13482,#3081);
#2237=LINE('',#13483,#3082);
#2238=LINE('',#13486,#3083);
#2239=LINE('',#13487,#3084);
#2240=LINE('',#13490,#3085);
#2241=LINE('',#13491,#3086);
#2242=LINE('',#13494,#3087);
#2243=LINE('',#13495,#3088);
#2244=LINE('',#13498,#3089);
#2245=LINE('',#13499,#3090);
#2246=LINE('',#13502,#3091);
#2247=LINE('',#13503,#3092);
#2248=LINE('',#13506,#3093);
#2249=LINE('',#13507,#3094);
#2250=LINE('',#13510,#3095);
#2251=LINE('',#13511,#3096);
#2252=LINE('',#13514,#3097);
#2253=LINE('',#13515,#3098);
#2254=LINE('',#13517,#3099);
#2255=LINE('',#13526,#3100);
#2256=LINE('',#13531,#3101);
#2257=LINE('',#13539,#3102);
#2258=LINE('',#13550,#3103);
#2259=LINE('',#13561,#3104);
#2260=LINE('',#13572,#3105);
#2261=LINE('',#13583,#3106);
#2262=LINE('',#13594,#3107);
#2263=LINE('',#13605,#3108);
#2264=LINE('',#13616,#3109);
#2265=LINE('',#13627,#3110);
#2266=LINE('',#13643,#3111);
#2267=LINE('',#13645,#3112);
#2268=LINE('',#13646,#3113);
#2269=LINE('',#13649,#3114);
#2270=LINE('',#13650,#3115);
#2271=LINE('',#13653,#3116);
#2272=LINE('',#13654,#3117);
#2273=LINE('',#13657,#3118);
#2274=LINE('',#13658,#3119);
#2275=LINE('',#13661,#3120);
#2276=LINE('',#13662,#3121);
#2277=LINE('',#13665,#3122);
#2278=LINE('',#13666,#3123);
#2279=LINE('',#13669,#3124);
#2280=LINE('',#13670,#3125);
#2281=LINE('',#13673,#3126);
#2282=LINE('',#13674,#3127);
#2283=LINE('',#13677,#3128);
#2284=LINE('',#13678,#3129);
#2285=LINE('',#13680,#3130);
#2286=LINE('',#13689,#3131);
#2287=LINE('',#13694,#3132);
#2288=LINE('',#13702,#3133);
#2289=LINE('',#13713,#3134);
#2290=LINE('',#13724,#3135);
#2291=LINE('',#13735,#3136);
#2292=LINE('',#13746,#3137);
#2293=LINE('',#13757,#3138);
#2294=LINE('',#13768,#3139);
#2295=LINE('',#13779,#3140);
#2296=LINE('',#13790,#3141);
#2297=LINE('',#13805,#3142);
#2298=LINE('',#13807,#3143);
#2299=LINE('',#13809,#3144);
#2300=LINE('',#13811,#3145);
#2301=LINE('',#13813,#3146);
#2302=LINE('',#13815,#3147);
#2303=LINE('',#13817,#3148);
#2304=LINE('',#13823,#3149);
#2305=LINE('',#13825,#3150);
#2306=LINE('',#13827,#3151);
#2307=LINE('',#13828,#3152);
#2308=LINE('',#13832,#3153);
#2309=LINE('',#13838,#3154);
#2310=LINE('',#13839,#3155);
#2311=LINE('',#13840,#3156);
#2312=LINE('',#13844,#3157);
#2313=LINE('',#13850,#3158);
#2314=LINE('',#13851,#3159);
#2315=LINE('',#13852,#3160);
#2316=LINE('',#13856,#3161);
#2317=LINE('',#13862,#3162);
#2318=LINE('',#13863,#3163);
#2319=LINE('',#13864,#3164);
#2320=LINE('',#13870,#3165);
#2321=LINE('',#13873,#3166);
#2322=LINE('',#13876,#3167);
#2323=LINE('',#13877,#3168);
#2324=LINE('',#13880,#3169);
#2325=LINE('',#13884,#3170);
#2326=LINE('',#13885,#3171);
#2327=LINE('',#13901,#3172);
#2328=LINE('',#13906,#3173);
#2329=LINE('',#13910,#3174);
#2330=LINE('',#13914,#3175);
#2331=LINE('',#13918,#3176);
#2332=LINE('',#13930,#3177);
#2333=LINE('',#13934,#3178);
#2334=LINE('',#13936,#3179);
#2335=LINE('',#13937,#3180);
#2336=LINE('',#13941,#3181);
#2337=LINE('',#13943,#3182);
#2338=LINE('',#13944,#3183);
#2339=LINE('',#13946,#3184);
#2340=LINE('',#13948,#3185);
#2341=LINE('',#13950,#3186);
#2342=LINE('',#13952,#3187);
#2343=LINE('',#13956,#3188);
#2344=LINE('',#13958,#3189);
#2345=LINE('',#13960,#3190);
#2346=LINE('',#13964,#3191);
#2347=LINE('',#13967,#3192);
#2348=LINE('',#13972,#3193);
#2349=LINE('',#13975,#3194);
#2350=LINE('',#13980,#3195);
#2351=LINE('',#13983,#3196);
#2352=LINE('',#13986,#3197);
#2353=LINE('',#13988,#3198);
#2354=LINE('',#13990,#3199);
#2355=LINE('',#13992,#3200);
#2356=LINE('',#13994,#3201);
#2357=LINE('',#14001,#3202);
#2358=LINE('',#14006,#3203);
#2359=LINE('',#14008,#3204);
#2360=LINE('',#14010,#3205);
#2361=LINE('',#14012,#3206);
#2362=LINE('',#14014,#3207);
#2363=LINE('',#14016,#3208);
#2364=LINE('',#14018,#3209);
#2365=LINE('',#14020,#3210);
#2366=LINE('',#14022,#3211);
#2367=LINE('',#14024,#3212);
#2368=LINE('',#14026,#3213);
#2369=LINE('',#14028,#3214);
#2370=LINE('',#14030,#3215);
#2371=LINE('',#14032,#3216);
#2372=LINE('',#14034,#3217);
#2373=LINE('',#14036,#3218);
#2374=LINE('',#14038,#3219);
#2375=LINE('',#14040,#3220);
#2376=LINE('',#14042,#3221);
#2377=LINE('',#14044,#3222);
#2378=LINE('',#14046,#3223);
#2379=LINE('',#14048,#3224);
#2380=LINE('',#14051,#3225);
#2381=LINE('',#14056,#3226);
#2382=LINE('',#14060,#3227);
#2383=LINE('',#14064,#3228);
#2384=LINE('',#14069,#3229);
#2385=LINE('',#14071,#3230);
#2386=LINE('',#14073,#3231);
#2387=LINE('',#14075,#3232);
#2388=LINE('',#14077,#3233);
#2389=LINE('',#14078,#3234);
#2390=LINE('',#14081,#3235);
#2391=LINE('',#14083,#3236);
#2392=LINE('',#14084,#3237);
#2393=LINE('',#14087,#3238);
#2394=LINE('',#14089,#3239);
#2395=LINE('',#14091,#3240);
#2396=LINE('',#14092,#3241);
#2397=LINE('',#14095,#3242);
#2398=LINE('',#14097,#3243);
#2399=LINE('',#14098,#3244);
#2400=LINE('',#14101,#3245);
#2401=LINE('',#14103,#3246);
#2402=LINE('',#14105,#3247);
#2403=LINE('',#14106,#3248);
#2404=LINE('',#14108,#3249);
#2405=LINE('',#14109,#3250);
#2406=LINE('',#14112,#3251);
#2407=LINE('',#14113,#3252);
#2408=LINE('',#14118,#3253);
#2409=LINE('',#14122,#3254);
#2410=LINE('',#14126,#3255);
#2411=LINE('',#14128,#3256);
#2412=LINE('',#14130,#3257);
#2413=LINE('',#14132,#3258);
#2414=LINE('',#14134,#3259);
#2415=LINE('',#14136,#3260);
#2416=LINE('',#14138,#3261);
#2417=LINE('',#14140,#3262);
#2418=LINE('',#14142,#3263);
#2419=LINE('',#14144,#3264);
#2420=LINE('',#14146,#3265);
#2421=LINE('',#14148,#3266);
#2422=LINE('',#14150,#3267);
#2423=LINE('',#14152,#3268);
#2424=LINE('',#14154,#3269);
#2425=LINE('',#14156,#3270);
#2426=LINE('',#14158,#3271);
#2427=LINE('',#14160,#3272);
#2428=LINE('',#14162,#3273);
#2429=LINE('',#14163,#3274);
#2430=LINE('',#14168,#3275);
#2431=LINE('',#14172,#3276);
#2432=LINE('',#14176,#3277);
#2433=LINE('',#14181,#3278);
#2434=LINE('',#14182,#3279);
#2435=LINE('',#14183,#3280);
#2436=LINE('',#14185,#3281);
#2437=LINE('',#14189,#3282);
#2438=LINE('',#14192,#3283);
#2439=LINE('',#14193,#3284);
#2440=LINE('',#14195,#3285);
#2441=LINE('',#14196,#3286);
#2442=LINE('',#14200,#3287);
#2443=LINE('',#14204,#3288);
#2444=LINE('',#14206,#3289);
#2445=LINE('',#14207,#3290);
#2446=LINE('',#14211,#3291);
#2447=LINE('',#14212,#3292);
#2448=LINE('',#14213,#3293);
#2449=LINE('',#14216,#3294);
#2450=LINE('',#14218,#3295);
#2451=LINE('',#14219,#3296);
#2452=LINE('',#14221,#3297);
#2453=LINE('',#14222,#3298);
#2454=LINE('',#14225,#3299);
#2455=LINE('',#14227,#3300);
#2456=LINE('',#14228,#3301);
#2457=LINE('',#14232,#3302);
#2458=LINE('',#14236,#3303);
#2459=LINE('',#14238,#3304);
#2460=LINE('',#14246,#3305);
#2461=LINE('',#14249,#3306);
#2462=LINE('',#14250,#3307);
#2463=LINE('',#14254,#3308);
#2464=LINE('',#14255,#3309);
#2465=LINE('',#14256,#3310);
#2466=LINE('',#14259,#3311);
#2467=LINE('',#14260,#3312);
#2468=LINE('',#14263,#3313);
#2469=LINE('',#14264,#3314);
#2470=LINE('',#14267,#3315);
#2471=LINE('',#14268,#3316);
#2472=LINE('',#14271,#3317);
#2473=LINE('',#14272,#3318);
#2474=LINE('',#14275,#3319);
#2475=LINE('',#14276,#3320);
#2476=LINE('',#14278,#3321);
#2477=LINE('',#14281,#3322);
#2478=LINE('',#14282,#3323);
#2479=LINE('',#14285,#3324);
#2480=LINE('',#14286,#3325);
#2481=LINE('',#14289,#3326);
#2482=LINE('',#14290,#3327);
#2483=LINE('',#14293,#3328);
#2484=LINE('',#14294,#3329);
#2485=LINE('',#14297,#3330);
#2486=LINE('',#14298,#3331);
#2487=LINE('',#14301,#3332);
#2488=LINE('',#14302,#3333);
#2489=LINE('',#14305,#3334);
#2490=LINE('',#14306,#3335);
#2491=LINE('',#14309,#3336);
#2492=LINE('',#14310,#3337);
#2493=LINE('',#14313,#3338);
#2494=LINE('',#14314,#3339);
#2495=LINE('',#14316,#3340);
#2496=LINE('',#14319,#3341);
#2497=LINE('',#14321,#3342);
#2498=LINE('',#14322,#3343);
#2499=LINE('',#14325,#3344);
#2500=LINE('',#14326,#3345);
#2501=LINE('',#14329,#3346);
#2502=LINE('',#14330,#3347);
#2503=LINE('',#14333,#3348);
#2504=LINE('',#14334,#3349);
#2505=LINE('',#14337,#3350);
#2506=LINE('',#14338,#3351);
#2507=LINE('',#14341,#3352);
#2508=LINE('',#14342,#3353);
#2509=LINE('',#14344,#3354);
#2510=LINE('',#14345,#3355);
#2511=LINE('',#14348,#3356);
#2512=LINE('',#14350,#3357);
#2513=LINE('',#14352,#3358);
#2514=LINE('',#14354,#3359);
#2515=LINE('',#14356,#3360);
#2516=LINE('',#14358,#3361);
#2517=LINE('',#14360,#3362);
#2518=LINE('',#14363,#3363);
#2519=LINE('',#14364,#3364);
#2520=LINE('',#14367,#3365);
#2521=LINE('',#14368,#3366);
#2522=LINE('',#14371,#3367);
#2523=LINE('',#14372,#3368);
#2524=LINE('',#14375,#3369);
#2525=LINE('',#14376,#3370);
#2526=LINE('',#14379,#3371);
#2527=LINE('',#14380,#3372);
#2528=LINE('',#14383,#3373);
#2529=LINE('',#14385,#3374);
#2530=LINE('',#14386,#3375);
#2531=LINE('',#14389,#3376);
#2532=LINE('',#14390,#3377);
#2533=LINE('',#14393,#3378);
#2534=LINE('',#14394,#3379);
#2535=LINE('',#14396,#3380);
#2536=LINE('',#14398,#3381);
#2537=LINE('',#14400,#3382);
#2538=LINE('',#14402,#3383);
#2539=LINE('',#14404,#3384);
#2540=LINE('',#14412,#3385);
#2541=LINE('',#14414,#3386);
#2542=LINE('',#14416,#3387);
#2543=LINE('',#14418,#3388);
#2544=LINE('',#14420,#3389);
#2545=LINE('',#14422,#3390);
#2546=LINE('',#14424,#3391);
#2547=LINE('',#14431,#3392);
#2548=LINE('',#14433,#3393);
#2549=LINE('',#14435,#3394);
#2550=LINE('',#14444,#3395);
#2551=LINE('',#14448,#3396);
#2552=LINE('',#14452,#3397);
#2553=LINE('',#14459,#3398);
#2554=LINE('',#14465,#3399);
#2555=LINE('',#14475,#3400);
#2556=LINE('',#14480,#3401);
#2557=LINE('',#14491,#3402);
#2558=LINE('',#14493,#3403);
#2559=LINE('',#14494,#3404);
#2560=LINE('',#14498,#3405);
#2561=LINE('',#14503,#3406);
#2562=LINE('',#14511,#3407);
#2563=LINE('',#14517,#3408);
#2564=LINE('',#14521,#3409);
#2565=LINE('',#14528,#3410);
#2566=LINE('',#14532,#3411);
#2567=LINE('',#14541,#3412);
#2568=LINE('',#14549,#3413);
#2569=LINE('',#14553,#3414);
#2570=LINE('',#14560,#3415);
#2571=LINE('',#14566,#3416);
#2572=LINE('',#14570,#3417);
#2573=LINE('',#14574,#3418);
#2574=LINE('',#14577,#3419);
#2575=LINE('',#14580,#3420);
#2576=LINE('',#14584,#3421);
#2577=LINE('',#14588,#3422);
#2578=LINE('',#14591,#3423);
#2579=LINE('',#14593,#3424);
#2580=LINE('',#14597,#3425);
#2581=LINE('',#14601,#3426);
#2582=LINE('',#14605,#3427);
#2583=LINE('',#14607,#3428);
#2584=LINE('',#14608,#3429);
#2585=LINE('',#14611,#3430);
#2586=LINE('',#14615,#3431);
#2587=LINE('',#14619,#3432);
#2588=LINE('',#14624,#3433);
#2589=LINE('',#14707,#3434);
#2590=LINE('',#14750,#3435);
#2591=LINE('',#14798,#3436);
#2592=LINE('',#14818,#3437);
#2593=LINE('',#14823,#3438);
#2594=LINE('',#14830,#3439);
#2595=LINE('',#14837,#3440);
#2596=LINE('',#14839,#3441);
#2597=LINE('',#14841,#3442);
#2598=LINE('',#14842,#3443);
#2599=LINE('',#14845,#3444);
#2600=LINE('',#14847,#3445);
#2601=LINE('',#14848,#3446);
#2602=LINE('',#14852,#3447);
#2603=LINE('',#14854,#3448);
#2604=LINE('',#14856,#3449);
#2605=LINE('',#14857,#3450);
#2606=LINE('',#14860,#3451);
#2607=LINE('',#14862,#3452);
#2608=LINE('',#14863,#3453);
#2609=LINE('',#14867,#3454);
#2610=LINE('',#14869,#3455);
#2611=LINE('',#14871,#3456);
#2612=LINE('',#14872,#3457);
#2613=LINE('',#14875,#3458);
#2614=LINE('',#14877,#3459);
#2615=LINE('',#14878,#3460);
#2616=LINE('',#14882,#3461);
#2617=LINE('',#14884,#3462);
#2618=LINE('',#14886,#3463);
#2619=LINE('',#14887,#3464);
#2620=LINE('',#14890,#3465);
#2621=LINE('',#14892,#3466);
#2622=LINE('',#14893,#3467);
#2623=LINE('',#14901,#3468);
#2624=LINE('',#14906,#3469);
#2625=LINE('',#14913,#3470);
#2626=LINE('',#14924,#3471);
#2627=LINE('',#14929,#3472);
#2628=LINE('',#14936,#3473);
#2629=LINE('',#14943,#3474);
#2630=LINE('',#14945,#3475);
#2631=LINE('',#14947,#3476);
#2632=LINE('',#14948,#3477);
#2633=LINE('',#14951,#3478);
#2634=LINE('',#14953,#3479);
#2635=LINE('',#14954,#3480);
#2636=LINE('',#14958,#3481);
#2637=LINE('',#14960,#3482);
#2638=LINE('',#14962,#3483);
#2639=LINE('',#14963,#3484);
#2640=LINE('',#14966,#3485);
#2641=LINE('',#14968,#3486);
#2642=LINE('',#14969,#3487);
#2643=LINE('',#14977,#3488);
#2644=LINE('',#14982,#3489);
#2645=LINE('',#14989,#3490);
#2646=LINE('',#14996,#3491);
#2647=LINE('',#14998,#3492);
#2648=LINE('',#15000,#3493);
#2649=LINE('',#15001,#3494);
#2650=LINE('',#15004,#3495);
#2651=LINE('',#15006,#3496);
#2652=LINE('',#15007,#3497);
#2653=LINE('',#15015,#3498);
#2654=LINE('',#15020,#3499);
#2655=LINE('',#15027,#3500);
#2656=LINE('',#15038,#3501);
#2657=LINE('',#15043,#3502);
#2658=LINE('',#15050,#3503);
#2659=LINE('',#15058,#3504);
#2660=LINE('',#15061,#3505);
#2661=LINE('',#15066,#3506);
#2662=LINE('',#15068,#3507);
#2663=LINE('',#15069,#3508);
#2664=LINE('',#15070,#3509);
#2665=LINE('',#15071,#3510);
#2666=LINE('',#15072,#3511);
#2667=LINE('',#15073,#3512);
#2668=LINE('',#15074,#3513);
#2669=LINE('',#15075,#3514);
#2670=LINE('',#15076,#3515);
#2671=LINE('',#15082,#3516);
#2672=LINE('',#15086,#3517);
#2673=LINE('',#15088,#3518);
#2674=LINE('',#15096,#3519);
#2675=LINE('',#15098,#3520);
#2676=LINE('',#15100,#3521);
#2677=LINE('',#15102,#3522);
#2678=LINE('',#15104,#3523);
#2679=LINE('',#15107,#3524);
#2680=LINE('',#15111,#3525);
#2681=LINE('',#15112,#3526);
#2682=LINE('',#15114,#3527);
#2683=LINE('',#15116,#3528);
#2684=LINE('',#15117,#3529);
#2685=LINE('',#15118,#3530);
#2686=LINE('',#15120,#3531);
#2687=LINE('',#15121,#3532);
#2688=LINE('',#15123,#3533);
#2689=LINE('',#15124,#3534);
#2690=LINE('',#15126,#3535);
#2691=LINE('',#15127,#3536);
#2692=LINE('',#15129,#3537);
#2693=LINE('',#15133,#3538);
#2694=LINE('',#15139,#3539);
#2695=LINE('',#15141,#3540);
#2696=LINE('',#15143,#3541);
#2697=LINE('',#15144,#3542);
#2698=LINE('',#15147,#3543);
#2699=LINE('',#15150,#3544);
#2700=LINE('',#15154,#3545);
#2701=LINE('',#15160,#3546);
#2702=LINE('',#15166,#3547);
#2703=LINE('',#15171,#3548);
#2704=LINE('',#15195,#3549);
#2705=LINE('',#15243,#3550);
#2706=LINE('',#15291,#3551);
#2707=LINE('',#15345,#3552);
#2708=LINE('',#15393,#3553);
#2709=LINE('',#15403,#3554);
#2710=LINE('',#15428,#3555);
#2711=LINE('',#15453,#3556);
#2712=LINE('',#15478,#3557);
#2713=LINE('',#16188,#3558);
#2714=LINE('',#16190,#3559);
#2715=LINE('',#16192,#3560);
#2716=LINE('',#16193,#3561);
#2717=LINE('',#16196,#3562);
#2718=LINE('',#16198,#3563);
#2719=LINE('',#16199,#3564);
#2720=LINE('',#16202,#3565);
#2721=LINE('',#16204,#3566);
#2722=LINE('',#16205,#3567);
#2723=LINE('',#16208,#3568);
#2724=LINE('',#16210,#3569);
#2725=LINE('',#16211,#3570);
#2726=LINE('',#16214,#3571);
#2727=LINE('',#16216,#3572);
#2728=LINE('',#16217,#3573);
#2729=LINE('',#16219,#3574);
#2730=LINE('',#16220,#3575);
#2731=LINE('',#16226,#3576);
#2732=LINE('',#16232,#3577);
#2733=LINE('',#16238,#3578);
#2734=LINE('',#16262,#3579);
#2735=LINE('',#16310,#3580);
#2736=LINE('',#16358,#3581);
#2737=LINE('',#16412,#3582);
#2738=LINE('',#16460,#3583);
#2739=LINE('',#16508,#3584);
#2740=LINE('',#16562,#3585);
#2741=LINE('',#16610,#3586);
#2742=LINE('',#16658,#3587);
#2743=LINE('',#16712,#3588);
#2744=LINE('',#16760,#3589);
#2745=LINE('',#16814,#3590);
#2746=LINE('',#16832,#3591);
#2747=LINE('',#16857,#3592);
#2748=LINE('',#16882,#3593);
#2749=LINE('',#16907,#3594);
#2750=LINE('',#16932,#3595);
#2751=LINE('',#16956,#3596);
#2752=LINE('',#16981,#3597);
#2753=LINE('',#17006,#3598);
#2754=LINE('',#17030,#3599);
#2755=LINE('',#17055,#3600);
#2756=LINE('',#17080,#3601);
#2757=LINE('',#18160,#3602);
#2758=LINE('',#18165,#3603);
#2759=LINE('',#18167,#3604);
#2760=LINE('',#18169,#3605);
#2761=LINE('',#18170,#3606);
#2762=LINE('',#18173,#3607);
#2763=LINE('',#18175,#3608);
#2764=LINE('',#18176,#3609);
#2765=LINE('',#18179,#3610);
#2766=LINE('',#18181,#3611);
#2767=LINE('',#18182,#3612);
#2768=LINE('',#18185,#3613);
#2769=LINE('',#18187,#3614);
#2770=LINE('',#18188,#3615);
#2771=LINE('',#18191,#3616);
#2772=LINE('',#18193,#3617);
#2773=LINE('',#18194,#3618);
#2774=LINE('',#18196,#3619);
#2775=LINE('',#18197,#3620);
#2776=LINE('',#18203,#3621);
#2777=LINE('',#18209,#3622);
#2778=LINE('',#18218,#3623);
#2779=LINE('',#18222,#3624);
#2780=LINE('',#18226,#3625);
#2781=VECTOR('',#9976,10.);
#2782=VECTOR('',#9977,10.);
#2783=VECTOR('',#9978,10.);
#2784=VECTOR('',#9981,10.);
#2785=VECTOR('',#9982,10.);
#2786=VECTOR('',#9983,10.);
#2787=VECTOR('',#9986,10.);
#2788=VECTOR('',#9987,10.);
#2789=VECTOR('',#9988,10.);
#2790=VECTOR('',#9991,10.);
#2791=VECTOR('',#9992,10.);
#2792=VECTOR('',#9993,10.);
#2793=VECTOR('',#9998,10.);
#2794=VECTOR('',#9999,10.);
#2795=VECTOR('',#10002,10.);
#2796=VECTOR('',#10003,10.);
#2797=VECTOR('',#10006,10.);
#2798=VECTOR('',#10007,10.);
#2799=VECTOR('',#10010,10.);
#2800=VECTOR('',#10011,10.);
#2801=VECTOR('',#10016,10.);
#2802=VECTOR('',#10017,10.);
#2803=VECTOR('',#10022,10.);
#2804=VECTOR('',#10023,10.);
#2805=VECTOR('',#10026,10.);
#2806=VECTOR('',#10027,10.);
#2807=VECTOR('',#10032,10.);
#2808=VECTOR('',#10033,10.);
#2809=VECTOR('',#10036,10.);
#2810=VECTOR('',#10053,2.5);
#2811=VECTOR('',#10058,2.5);
#2812=VECTOR('',#10063,2.5);
#2813=VECTOR('',#10066,10.);
#2814=VECTOR('',#10077,10.);
#2815=VECTOR('',#10078,10.);
#2816=VECTOR('',#10079,10.);
#2817=VECTOR('',#10082,10.);
#2818=VECTOR('',#10083,10.);
#2819=VECTOR('',#10084,10.);
#2820=VECTOR('',#10089,10.);
#2821=VECTOR('',#10090,10.);
#2822=VECTOR('',#10093,10.);
#2823=VECTOR('',#10094,10.);
#2824=VECTOR('',#10097,10.);
#2825=VECTOR('',#10098,10.);
#2826=VECTOR('',#10099,10.);
#2827=VECTOR('',#10102,10.);
#2828=VECTOR('',#10103,10.);
#2829=VECTOR('',#10104,10.);
#2830=VECTOR('',#10109,10.);
#2831=VECTOR('',#10110,10.);
#2832=VECTOR('',#10113,10.);
#2833=VECTOR('',#10114,10.);
#2834=VECTOR('',#10117,10.);
#2835=VECTOR('',#10118,10.);
#2836=VECTOR('',#10121,10.);
#2837=VECTOR('',#10122,10.);
#2838=VECTOR('',#10127,10.);
#2839=VECTOR('',#10128,10.);
#2840=VECTOR('',#10133,10.);
#2841=VECTOR('',#10134,10.);
#2842=VECTOR('',#10137,10.);
#2843=VECTOR('',#10146,10.);
#2844=VECTOR('',#10157,10.);
#2845=VECTOR('',#10158,10.);
#2846=VECTOR('',#10159,10.);
#2847=VECTOR('',#10160,10.);
#2848=VECTOR('',#10165,10.);
#2849=VECTOR('',#10170,10.);
#2850=VECTOR('',#10171,10.);
#2851=VECTOR('',#10172,10.);
#2852=VECTOR('',#10177,10.);
#2853=VECTOR('',#10182,10.);
#2854=VECTOR('',#10183,10.);
#2855=VECTOR('',#10184,10.);
#2856=VECTOR('',#10189,10.);
#2857=VECTOR('',#10194,10.);
#2858=VECTOR('',#10195,10.);
#2859=VECTOR('',#10196,10.);
#2860=VECTOR('',#10205,10.);
#2861=VECTOR('',#10208,10.);
#2862=VECTOR('',#10211,10.);
#2863=VECTOR('',#10212,10.);
#2864=VECTOR('',#10215,10.);
#2865=VECTOR('',#10220,10.);
#2866=VECTOR('',#10221,10.);
#2867=VECTOR('',#10236,10.);
#2868=VECTOR('',#10237,10.);
#2869=VECTOR('',#10238,10.);
#2870=VECTOR('',#10239,10.);
#2871=VECTOR('',#10242,10.);
#2872=VECTOR('',#10247,10.);
#2873=VECTOR('',#10248,10.);
#2874=VECTOR('',#10251,10.);
#2875=VECTOR('',#10256,10.);
#2876=VECTOR('',#10257,10.);
#2877=VECTOR('',#10260,10.);
#2878=VECTOR('',#10267,10.);
#2879=VECTOR('',#10268,10.);
#2880=VECTOR('',#10269,10.);
#2881=VECTOR('',#10270,10.);
#2882=VECTOR('',#10271,10.);
#2883=VECTOR('',#10280,10.);
#2884=VECTOR('',#10283,10.);
#2885=VECTOR('',#10286,10.);
#2886=VECTOR('',#10289,10.);
#2887=VECTOR('',#10290,10.);
#2888=VECTOR('',#10293,10.);
#2889=VECTOR('',#10298,10.);
#2890=VECTOR('',#10299,10.);
#2891=VECTOR('',#10300,10.);
#2892=VECTOR('',#10301,10.);
#2893=VECTOR('',#10302,10.);
#2894=VECTOR('',#10303,10.);
#2895=VECTOR('',#10304,10.);
#2896=VECTOR('',#10305,10.);
#2897=VECTOR('',#10306,10.);
#2898=VECTOR('',#10307,10.);
#2899=VECTOR('',#10310,10.);
#2900=VECTOR('',#10311,10.);
#2901=VECTOR('',#10314,10.);
#2902=VECTOR('',#10319,3.27928932188134);
#2903=VECTOR('',#10326,10.);
#2904=VECTOR('',#10329,10.);
#2905=VECTOR('',#10332,10.);
#2906=VECTOR('',#10333,10.);
#2907=VECTOR('',#10334,10.);
#2908=VECTOR('',#10335,10.);
#2909=VECTOR('',#10338,2.475);
#2910=VECTOR('',#10345,3.27928932188134);
#2911=VECTOR('',#10352,10.);
#2912=VECTOR('',#10353,10.);
#2913=VECTOR('',#10356,10.);
#2914=VECTOR('',#10357,10.);
#2915=VECTOR('',#10360,2.475);
#2916=VECTOR('',#10367,3.27928932188134);
#2917=VECTOR('',#10372,10.);
#2918=VECTOR('',#10373,10.);
#2919=VECTOR('',#10374,10.);
#2920=VECTOR('',#10377,10.);
#2921=VECTOR('',#10380,10.);
#2922=VECTOR('',#10381,10.);
#2923=VECTOR('',#10382,10.);
#2924=VECTOR('',#10383,10.);
#2925=VECTOR('',#10384,10.);
#2926=VECTOR('',#10385,10.);
#2927=VECTOR('',#10386,10.);
#2928=VECTOR('',#10387,10.);
#2929=VECTOR('',#10388,10.);
#2930=VECTOR('',#10389,10.);
#2931=VECTOR('',#10390,10.);
#2932=VECTOR('',#10391,10.);
#2933=VECTOR('',#10392,10.);
#2934=VECTOR('',#10393,10.);
#2935=VECTOR('',#10394,10.);
#2936=VECTOR('',#10395,10.);
#2937=VECTOR('',#10396,10.);
#2938=VECTOR('',#10397,10.);
#2939=VECTOR('',#10398,10.);
#2940=VECTOR('',#10399,10.);
#2941=VECTOR('',#10400,10.);
#2942=VECTOR('',#10401,10.);
#2943=VECTOR('',#10402,10.);
#2944=VECTOR('',#10403,10.);
#2945=VECTOR('',#10404,10.);
#2946=VECTOR('',#10405,10.);
#2947=VECTOR('',#10406,10.);
#2948=VECTOR('',#10407,10.);
#2949=VECTOR('',#10408,10.);
#2950=VECTOR('',#10409,10.);
#2951=VECTOR('',#10410,10.);
#2952=VECTOR('',#10411,10.);
#2953=VECTOR('',#10412,10.);
#2954=VECTOR('',#10413,10.);
#2955=VECTOR('',#10414,10.);
#2956=VECTOR('',#10415,10.);
#2957=VECTOR('',#10416,10.);
#2958=VECTOR('',#10417,10.);
#2959=VECTOR('',#10418,10.);
#2960=VECTOR('',#10419,10.);
#2961=VECTOR('',#10420,10.);
#2962=VECTOR('',#10421,10.);
#2963=VECTOR('',#10422,10.);
#2964=VECTOR('',#10423,10.);
#2965=VECTOR('',#10424,10.);
#2966=VECTOR('',#10425,10.);
#2967=VECTOR('',#10428,10.);
#2968=VECTOR('',#10429,10.);
#2969=VECTOR('',#10430,10.);
#2970=VECTOR('',#10431,10.);
#2971=VECTOR('',#10432,10.);
#2972=VECTOR('',#10433,10.);
#2973=VECTOR('',#10434,10.);
#2974=VECTOR('',#10435,10.);
#2975=VECTOR('',#10436,10.);
#2976=VECTOR('',#10437,10.);
#2977=VECTOR('',#10440,2.475);
#2978=VECTOR('',#10447,3.27928932188134);
#2979=VECTOR('',#10450,2.475);
#2980=VECTOR('',#10455,10.);
#2981=VECTOR('',#10456,10.);
#2982=VECTOR('',#10457,10.);
#2983=VECTOR('',#10458,10.);
#2984=VECTOR('',#10461,10.);
#2985=VECTOR('',#10462,10.);
#2986=VECTOR('',#10465,10.);
#2987=VECTOR('',#10466,10.);
#2988=VECTOR('',#10471,10.);
#2989=VECTOR('',#10474,10.);
#2990=VECTOR('',#10475,10.);
#2991=VECTOR('',#10482,10.);
#2992=VECTOR('',#10485,10.);
#2993=VECTOR('',#10488,10.);
#2994=VECTOR('',#10493,10.);
#2995=VECTOR('',#10494,10.);
#2996=VECTOR('',#10497,10.);
#2997=VECTOR('',#10498,10.);
#2998=VECTOR('',#10503,10.);
#2999=VECTOR('',#10504,10.);
#3000=VECTOR('',#10507,10.);
#3001=VECTOR('',#10508,10.);
#3002=VECTOR('',#10511,10.);
#3003=VECTOR('',#10512,10.);
#3004=VECTOR('',#10515,10.);
#3005=VECTOR('',#10516,10.);
#3006=VECTOR('',#10519,10.);
#3007=VECTOR('',#10520,10.);
#3008=VECTOR('',#10523,10.);
#3009=VECTOR('',#10524,10.);
#3010=VECTOR('',#10527,10.);
#3011=VECTOR('',#10532,10.);
#3012=VECTOR('',#10533,10.);
#3013=VECTOR('',#10536,10.);
#3014=VECTOR('',#10537,10.);
#3015=VECTOR('',#10540,10.);
#3016=VECTOR('',#10541,10.);
#3017=VECTOR('',#10544,10.);
#3018=VECTOR('',#10545,10.);
#3019=VECTOR('',#10548,10.);
#3020=VECTOR('',#10549,10.);
#3021=VECTOR('',#10552,10.);
#3022=VECTOR('',#10553,10.);
#3023=VECTOR('',#10556,10.);
#3024=VECTOR('',#10559,10.);
#3025=VECTOR('',#10560,10.);
#3026=VECTOR('',#10561,10.);
#3027=VECTOR('',#10562,10.);
#3028=VECTOR('',#10563,10.);
#3029=VECTOR('',#10566,10.);
#3030=VECTOR('',#10567,10.);
#3031=VECTOR('',#10568,10.);
#3032=VECTOR('',#10571,10.);
#3033=VECTOR('',#10572,10.);
#3034=VECTOR('',#10575,10.);
#3035=VECTOR('',#10576,10.);
#3036=VECTOR('',#10579,10.);
#3037=VECTOR('',#10580,10.);
#3038=VECTOR('',#10583,10.);
#3039=VECTOR('',#10584,10.);
#3040=VECTOR('',#10587,10.);
#3041=VECTOR('',#10588,10.);
#3042=VECTOR('',#10591,10.);
#3043=VECTOR('',#10592,10.);
#3044=VECTOR('',#10595,10.);
#3045=VECTOR('',#10596,10.);
#3046=VECTOR('',#10599,10.);
#3047=VECTOR('',#10600,10.);
#3048=VECTOR('',#10603,10.);
#3049=VECTOR('',#10608,10.);
#3050=VECTOR('',#10609,10.);
#3051=VECTOR('',#10610,10.);
#3052=VECTOR('',#10613,10.);
#3053=VECTOR('',#10614,10.);
#3054=VECTOR('',#10617,10.);
#3055=VECTOR('',#10618,10.);
#3056=VECTOR('',#10621,10.);
#3057=VECTOR('',#10622,10.);
#3058=VECTOR('',#10625,10.);
#3059=VECTOR('',#10626,10.);
#3060=VECTOR('',#10629,10.);
#3061=VECTOR('',#10630,10.);
#3062=VECTOR('',#10633,10.);
#3063=VECTOR('',#10634,10.);
#3064=VECTOR('',#10637,10.);
#3065=VECTOR('',#10638,10.);
#3066=VECTOR('',#10641,10.);
#3067=VECTOR('',#10642,10.);
#3068=VECTOR('',#10645,10.);
#3069=VECTOR('',#10648,10.);
#3070=VECTOR('',#10649,10.);
#3071=VECTOR('',#10650,10.);
#3072=VECTOR('',#10651,10.);
#3073=VECTOR('',#10652,10.);
#3074=VECTOR('',#10653,10.);
#3075=VECTOR('',#10654,10.);
#3076=VECTOR('',#10655,10.);
#3077=VECTOR('',#10656,10.);
#3078=VECTOR('',#10657,10.);
#3079=VECTOR('',#10658,10.);
#3080=VECTOR('',#10663,10.);
#3081=VECTOR('',#10664,10.);
#3082=VECTOR('',#10665,10.);
#3083=VECTOR('',#10668,10.);
#3084=VECTOR('',#10669,10.);
#3085=VECTOR('',#10672,10.);
#3086=VECTOR('',#10673,10.);
#3087=VECTOR('',#10676,10.);
#3088=VECTOR('',#10677,10.);
#3089=VECTOR('',#10680,10.);
#3090=VECTOR('',#10681,10.);
#3091=VECTOR('',#10684,10.);
#3092=VECTOR('',#10685,10.);
#3093=VECTOR('',#10688,10.);
#3094=VECTOR('',#10689,10.);
#3095=VECTOR('',#10692,10.);
#3096=VECTOR('',#10693,10.);
#3097=VECTOR('',#10696,10.);
#3098=VECTOR('',#10697,10.);
#3099=VECTOR('',#10700,10.);
#3100=VECTOR('',#10703,10.);
#3101=VECTOR('',#10704,10.);
#3102=VECTOR('',#10705,10.);
#3103=VECTOR('',#10706,10.);
#3104=VECTOR('',#10707,10.);
#3105=VECTOR('',#10708,10.);
#3106=VECTOR('',#10709,10.);
#3107=VECTOR('',#10710,10.);
#3108=VECTOR('',#10711,10.);
#3109=VECTOR('',#10712,10.);
#3110=VECTOR('',#10713,10.);
#3111=VECTOR('',#10718,10.);
#3112=VECTOR('',#10719,10.);
#3113=VECTOR('',#10720,10.);
#3114=VECTOR('',#10723,10.);
#3115=VECTOR('',#10724,10.);
#3116=VECTOR('',#10727,10.);
#3117=VECTOR('',#10728,10.);
#3118=VECTOR('',#10731,10.);
#3119=VECTOR('',#10732,10.);
#3120=VECTOR('',#10735,10.);
#3121=VECTOR('',#10736,10.);
#3122=VECTOR('',#10739,10.);
#3123=VECTOR('',#10740,10.);
#3124=VECTOR('',#10743,10.);
#3125=VECTOR('',#10744,10.);
#3126=VECTOR('',#10747,10.);
#3127=VECTOR('',#10748,10.);
#3128=VECTOR('',#10751,10.);
#3129=VECTOR('',#10752,10.);
#3130=VECTOR('',#10755,10.);
#3131=VECTOR('',#10758,10.);
#3132=VECTOR('',#10759,10.);
#3133=VECTOR('',#10760,10.);
#3134=VECTOR('',#10761,10.);
#3135=VECTOR('',#10762,10.);
#3136=VECTOR('',#10763,10.);
#3137=VECTOR('',#10764,10.);
#3138=VECTOR('',#10765,10.);
#3139=VECTOR('',#10766,10.);
#3140=VECTOR('',#10767,10.);
#3141=VECTOR('',#10768,10.);
#3142=VECTOR('',#10773,1.7);
#3143=VECTOR('',#10776,1.7);
#3144=VECTOR('',#10779,1.7);
#3145=VECTOR('',#10782,1.7);
#3146=VECTOR('',#10785,6.5);
#3147=VECTOR('',#10788,10.);
#3148=VECTOR('',#10791,10.);
#3149=VECTOR('',#10798,10.);
#3150=VECTOR('',#10799,10.);
#3151=VECTOR('',#10800,10.);
#3152=VECTOR('',#10801,10.);
#3153=VECTOR('',#10804,10.);
#3154=VECTOR('',#10811,10.);
#3155=VECTOR('',#10812,10.);
#3156=VECTOR('',#10813,10.);
#3157=VECTOR('',#10816,10.);
#3158=VECTOR('',#10823,10.);
#3159=VECTOR('',#10824,10.);
#3160=VECTOR('',#10825,10.);
#3161=VECTOR('',#10828,10.);
#3162=VECTOR('',#10835,10.);
#3163=VECTOR('',#10836,10.);
#3164=VECTOR('',#10837,10.);
#3165=VECTOR('',#10846,10.);
#3166=VECTOR('',#10849,10.);
#3167=VECTOR('',#10852,10.);
#3168=VECTOR('',#10853,10.);
#3169=VECTOR('',#10856,10.);
#3170=VECTOR('',#10861,10.);
#3171=VECTOR('',#10862,10.);
#3172=VECTOR('',#10879,3.27928932188134);
#3173=VECTOR('',#10884,10.);
#3174=VECTOR('',#10887,10.);
#3175=VECTOR('',#10890,10.);
#3176=VECTOR('',#10893,10.);
#3177=VECTOR('',#10906,2.475);
#3178=VECTOR('',#10911,10.);
#3179=VECTOR('',#10912,10.);
#3180=VECTOR('',#10913,10.);
#3181=VECTOR('',#10918,10.);
#3182=VECTOR('',#10921,10.);
#3183=VECTOR('',#10922,10.);
#3184=VECTOR('',#10925,10.);
#3185=VECTOR('',#10928,10.);
#3186=VECTOR('',#10931,10.);
#3187=VECTOR('',#10934,10.);
#3188=VECTOR('',#10941,10.);
#3189=VECTOR('',#10944,10.);
#3190=VECTOR('',#10947,10.);
#3191=VECTOR('',#10952,3.27928932188135);
#3192=VECTOR('',#10955,2.475);
#3193=VECTOR('',#10962,3.27928932188135);
#3194=VECTOR('',#10965,2.475);
#3195=VECTOR('',#10972,3.27928932188134);
#3196=VECTOR('',#10975,2.475);
#3197=VECTOR('',#10980,1.7);
#3198=VECTOR('',#10983,1.7);
#3199=VECTOR('',#10986,1.7);
#3200=VECTOR('',#10989,1.7);
#3201=VECTOR('',#10992,6.5);
#3202=VECTOR('',#11001,1.8);
#3203=VECTOR('',#11006,10.);
#3204=VECTOR('',#11007,10.);
#3205=VECTOR('',#11008,10.);
#3206=VECTOR('',#11009,10.);
#3207=VECTOR('',#11010,10.);
#3208=VECTOR('',#11011,10.);
#3209=VECTOR('',#11012,10.);
#3210=VECTOR('',#11013,10.);
#3211=VECTOR('',#11014,10.);
#3212=VECTOR('',#11015,10.);
#3213=VECTOR('',#11016,10.);
#3214=VECTOR('',#11017,10.);
#3215=VECTOR('',#11018,10.);
#3216=VECTOR('',#11019,10.);
#3217=VECTOR('',#11020,10.);
#3218=VECTOR('',#11021,10.);
#3219=VECTOR('',#11022,10.);
#3220=VECTOR('',#11023,10.);
#3221=VECTOR('',#11024,10.);
#3222=VECTOR('',#11025,10.);
#3223=VECTOR('',#11026,10.);
#3224=VECTOR('',#11027,10.);
#3225=VECTOR('',#11030,10.);
#3226=VECTOR('',#11035,1.55);
#3227=VECTOR('',#11040,1.8);
#3228=VECTOR('',#11045,1.55);
#3229=VECTOR('',#11050,10.);
#3230=VECTOR('',#11051,10.);
#3231=VECTOR('',#11052,10.);
#3232=VECTOR('',#11053,10.);
#3233=VECTOR('',#11054,10.);
#3234=VECTOR('',#11055,10.);
#3235=VECTOR('',#11058,10.);
#3236=VECTOR('',#11059,10.);
#3237=VECTOR('',#11060,10.);
#3238=VECTOR('',#11063,10.);
#3239=VECTOR('',#11064,10.);
#3240=VECTOR('',#11065,10.);
#3241=VECTOR('',#11066,10.);
#3242=VECTOR('',#11069,10.);
#3243=VECTOR('',#11070,10.);
#3244=VECTOR('',#11071,10.);
#3245=VECTOR('',#11074,10.);
#3246=VECTOR('',#11075,10.);
#3247=VECTOR('',#11076,10.);
#3248=VECTOR('',#11077,10.);
#3249=VECTOR('',#11080,10.);
#3250=VECTOR('',#11081,10.);
#3251=VECTOR('',#11084,10.);
#3252=VECTOR('',#11085,10.);
#3253=VECTOR('',#11090,1.8);
#3254=VECTOR('',#11095,10.);
#3255=VECTOR('',#11098,10.);
#3256=VECTOR('',#11099,10.);
#3257=VECTOR('',#11100,10.);
#3258=VECTOR('',#11101,10.);
#3259=VECTOR('',#11102,10.);
#3260=VECTOR('',#11103,10.);
#3261=VECTOR('',#11104,10.);
#3262=VECTOR('',#11105,10.);
#3263=VECTOR('',#11106,10.);
#3264=VECTOR('',#11107,10.);
#3265=VECTOR('',#11108,10.);
#3266=VECTOR('',#11109,10.);
#3267=VECTOR('',#11110,10.);
#3268=VECTOR('',#11111,10.);
#3269=VECTOR('',#11112,10.);
#3270=VECTOR('',#11113,10.);
#3271=VECTOR('',#11114,10.);
#3272=VECTOR('',#11115,10.);
#3273=VECTOR('',#11116,10.);
#3274=VECTOR('',#11117,10.);
#3275=VECTOR('',#11122,1.55);
#3276=VECTOR('',#11127,1.8);
#3277=VECTOR('',#11132,1.55);
#3278=VECTOR('',#11137,10.);
#3279=VECTOR('',#11138,10.);
#3280=VECTOR('',#11139,10.);
#3281=VECTOR('',#11142,10.);
#3282=VECTOR('',#11147,10.);
#3283=VECTOR('',#11150,10.);
#3284=VECTOR('',#11151,10.);
#3285=VECTOR('',#11154,10.);
#3286=VECTOR('',#11155,10.);
#3287=VECTOR('',#11160,10.);
#3288=VECTOR('',#11165,10.);
#3289=VECTOR('',#11166,10.);
#3290=VECTOR('',#11167,10.);
#3291=VECTOR('',#11170,10.);
#3292=VECTOR('',#11171,10.);
#3293=VECTOR('',#11172,10.);
#3294=VECTOR('',#11175,10.);
#3295=VECTOR('',#11176,10.);
#3296=VECTOR('',#11177,10.);
#3297=VECTOR('',#11180,10.);
#3298=VECTOR('',#11181,10.);
#3299=VECTOR('',#11184,10.);
#3300=VECTOR('',#11185,10.);
#3301=VECTOR('',#11186,10.);
#3302=VECTOR('',#11191,10.);
#3303=VECTOR('',#11196,10.);
#3304=VECTOR('',#11199,10.);
#3305=VECTOR('',#11208,10.);
#3306=VECTOR('',#11211,10.);
#3307=VECTOR('',#11212,10.);
#3308=VECTOR('',#11215,10.);
#3309=VECTOR('',#11216,10.);
#3310=VECTOR('',#11217,10.);
#3311=VECTOR('',#11220,10.);
#3312=VECTOR('',#11221,10.);
#3313=VECTOR('',#11224,10.);
#3314=VECTOR('',#11225,10.);
#3315=VECTOR('',#11228,10.);
#3316=VECTOR('',#11229,10.);
#3317=VECTOR('',#11232,10.);
#3318=VECTOR('',#11233,10.);
#3319=VECTOR('',#11236,10.);
#3320=VECTOR('',#11237,10.);
#3321=VECTOR('',#11240,10.);
#3322=VECTOR('',#11243,10.);
#3323=VECTOR('',#11244,10.);
#3324=VECTOR('',#11247,10.);
#3325=VECTOR('',#11248,10.);
#3326=VECTOR('',#11251,10.);
#3327=VECTOR('',#11252,10.);
#3328=VECTOR('',#11255,10.);
#3329=VECTOR('',#11256,10.);
#3330=VECTOR('',#11259,10.);
#3331=VECTOR('',#11260,10.);
#3332=VECTOR('',#11263,10.);
#3333=VECTOR('',#11264,10.);
#3334=VECTOR('',#11267,10.);
#3335=VECTOR('',#11268,10.);
#3336=VECTOR('',#11271,10.);
#3337=VECTOR('',#11272,10.);
#3338=VECTOR('',#11275,10.);
#3339=VECTOR('',#11276,10.);
#3340=VECTOR('',#11279,10.);
#3341=VECTOR('',#11282,10.);
#3342=VECTOR('',#11283,10.);
#3343=VECTOR('',#11284,10.);
#3344=VECTOR('',#11287,10.);
#3345=VECTOR('',#11288,10.);
#3346=VECTOR('',#11291,10.);
#3347=VECTOR('',#11292,10.);
#3348=VECTOR('',#11295,10.);
#3349=VECTOR('',#11296,10.);
#3350=VECTOR('',#11299,10.);
#3351=VECTOR('',#11300,10.);
#3352=VECTOR('',#11303,10.);
#3353=VECTOR('',#11304,10.);
#3354=VECTOR('',#11307,10.);
#3355=VECTOR('',#11308,10.);
#3356=VECTOR('',#11313,10.);
#3357=VECTOR('',#11316,10.);
#3358=VECTOR('',#11319,10.);
#3359=VECTOR('',#11322,10.);
#3360=VECTOR('',#11325,10.);
#3361=VECTOR('',#11328,10.);
#3362=VECTOR('',#11331,10.);
#3363=VECTOR('',#11334,10.);
#3364=VECTOR('',#11335,10.);
#3365=VECTOR('',#11338,10.);
#3366=VECTOR('',#11339,10.);
#3367=VECTOR('',#11342,10.);
#3368=VECTOR('',#11343,10.);
#3369=VECTOR('',#11346,10.);
#3370=VECTOR('',#11347,10.);
#3371=VECTOR('',#11350,10.);
#3372=VECTOR('',#11351,10.);
#3373=VECTOR('',#11354,10.);
#3374=VECTOR('',#11355,10.);
#3375=VECTOR('',#11356,10.);
#3376=VECTOR('',#11359,10.);
#3377=VECTOR('',#11360,10.);
#3378=VECTOR('',#11363,10.);
#3379=VECTOR('',#11364,10.);
#3380=VECTOR('',#11367,10.);
#3381=VECTOR('',#11370,10.);
#3382=VECTOR('',#11373,10.);
#3383=VECTOR('',#11376,10.);
#3384=VECTOR('',#11379,10.);
#3385=VECTOR('',#11388,10.);
#3386=VECTOR('',#11391,10.);
#3387=VECTOR('',#11394,10.);
#3388=VECTOR('',#11397,10.);
#3389=VECTOR('',#11400,10.);
#3390=VECTOR('',#11403,10.);
#3391=VECTOR('',#11406,10.);
#3392=VECTOR('',#11419,2.5);
#3393=VECTOR('',#11422,2.5);
#3394=VECTOR('',#11425,2.5);
#3395=VECTOR('',#11438,13.65);
#3396=VECTOR('',#11443,13.9);
#3397=VECTOR('',#11448,13.65);
#3398=VECTOR('',#11457,13.65);
#3399=VECTOR('',#11464,13.9);
#3400=VECTOR('',#11471,10.);
#3401=VECTOR('',#11472,10.);
#3402=VECTOR('',#11487,10.);
#3403=VECTOR('',#11490,10.);
#3404=VECTOR('',#11491,10.);
#3405=VECTOR('',#11496,5.);
#3406=VECTOR('',#11503,13.65);
#3407=VECTOR('',#11512,13.725);
#3408=VECTOR('',#11521,13.9);
#3409=VECTOR('',#11526,13.65);
#3410=VECTOR('',#11535,5.);
#3411=VECTOR('',#11540,4.75);
#3412=VECTOR('',#11551,8.35);
#3413=VECTOR('',#11562,8.5);
#3414=VECTOR('',#11567,5.025);
#3415=VECTOR('',#11576,6.5);
#3416=VECTOR('',#11583,10.);
#3417=VECTOR('',#11586,10.);
#3418=VECTOR('',#11591,10.);
#3419=VECTOR('',#11594,10.);
#3420=VECTOR('',#11597,10.);
#3421=VECTOR('',#11600,10.);
#3422=VECTOR('',#11605,10.);
#3423=VECTOR('',#11608,10.);
#3424=VECTOR('',#11611,10.);
#3425=VECTOR('',#11614,10.);
#3426=VECTOR('',#11617,10.);
#3427=VECTOR('',#11622,10.);
#3428=VECTOR('',#11623,10.);
#3429=VECTOR('',#11624,10.);
#3430=VECTOR('',#11627,10.);
#3431=VECTOR('',#11630,10.);
#3432=VECTOR('',#11635,10.);
#3433=VECTOR('',#11642,10.);
#3434=VECTOR('',#11643,10.);
#3435=VECTOR('',#11646,2.05);
#3436=VECTOR('',#11657,10.);
#3437=VECTOR('',#11676,10.);
#3438=VECTOR('',#11677,10.);
#3439=VECTOR('',#11680,10.);
#3440=VECTOR('',#11683,10.);
#3441=VECTOR('',#11684,10.);
#3442=VECTOR('',#11685,10.);
#3443=VECTOR('',#11686,10.);
#3444=VECTOR('',#11689,10.);
#3445=VECTOR('',#11690,10.);
#3446=VECTOR('',#11691,10.);
#3447=VECTOR('',#11694,10.);
#3448=VECTOR('',#11695,10.);
#3449=VECTOR('',#11696,10.);
#3450=VECTOR('',#11697,10.);
#3451=VECTOR('',#11700,10.);
#3452=VECTOR('',#11701,10.);
#3453=VECTOR('',#11702,10.);
#3454=VECTOR('',#11705,10.);
#3455=VECTOR('',#11706,10.);
#3456=VECTOR('',#11707,10.);
#3457=VECTOR('',#11708,10.);
#3458=VECTOR('',#11711,10.);
#3459=VECTOR('',#11712,10.);
#3460=VECTOR('',#11713,10.);
#3461=VECTOR('',#11716,10.);
#3462=VECTOR('',#11717,10.);
#3463=VECTOR('',#11718,10.);
#3464=VECTOR('',#11719,10.);
#3465=VECTOR('',#11722,10.);
#3466=VECTOR('',#11723,10.);
#3467=VECTOR('',#11724,10.);
#3468=VECTOR('',#11727,10.);
#3469=VECTOR('',#11728,10.);
#3470=VECTOR('',#11731,10.);
#3471=VECTOR('',#11734,10.);
#3472=VECTOR('',#11735,10.);
#3473=VECTOR('',#11738,10.);
#3474=VECTOR('',#11741,10.);
#3475=VECTOR('',#11742,10.);
#3476=VECTOR('',#11743,10.);
#3477=VECTOR('',#11744,10.);
#3478=VECTOR('',#11747,10.);
#3479=VECTOR('',#11748,10.);
#3480=VECTOR('',#11749,10.);
#3481=VECTOR('',#11752,10.);
#3482=VECTOR('',#11753,10.);
#3483=VECTOR('',#11754,10.);
#3484=VECTOR('',#11755,10.);
#3485=VECTOR('',#11758,10.);
#3486=VECTOR('',#11759,10.);
#3487=VECTOR('',#11760,10.);
#3488=VECTOR('',#11763,10.);
#3489=VECTOR('',#11764,10.);
#3490=VECTOR('',#11767,10.);
#3491=VECTOR('',#11770,10.);
#3492=VECTOR('',#11771,10.);
#3493=VECTOR('',#11772,10.);
#3494=VECTOR('',#11773,10.);
#3495=VECTOR('',#11776,10.);
#3496=VECTOR('',#11777,10.);
#3497=VECTOR('',#11778,10.);
#3498=VECTOR('',#11781,10.);
#3499=VECTOR('',#11782,10.);
#3500=VECTOR('',#11785,10.);
#3501=VECTOR('',#11788,10.);
#3502=VECTOR('',#11789,10.);
#3503=VECTOR('',#11792,10.);
#3504=VECTOR('',#11797,10.);
#3505=VECTOR('',#11800,10.);
#3506=VECTOR('',#11807,10.);
#3507=VECTOR('',#11808,10.);
#3508=VECTOR('',#11809,10.);
#3509=VECTOR('',#11810,10.);
#3510=VECTOR('',#11811,10.);
#3511=VECTOR('',#11812,10.);
#3512=VECTOR('',#11813,10.);
#3513=VECTOR('',#11814,10.);
#3514=VECTOR('',#11815,10.);
#3515=VECTOR('',#11816,10.);
#3516=VECTOR('',#11825,10.);
#3517=VECTOR('',#11832,10.);
#3518=VECTOR('',#11835,10.);
#3519=VECTOR('',#11848,10.);
#3520=VECTOR('',#11851,10.);
#3521=VECTOR('',#11854,10.);
#3522=VECTOR('',#11857,10.);
#3523=VECTOR('',#11860,10.);
#3524=VECTOR('',#11863,10.);
#3525=VECTOR('',#11870,10.);
#3526=VECTOR('',#11871,10.);
#3527=VECTOR('',#11874,10.);
#3528=VECTOR('',#11875,10.);
#3529=VECTOR('',#11876,10.);
#3530=VECTOR('',#11877,10.);
#3531=VECTOR('',#11880,10.);
#3532=VECTOR('',#11881,10.);
#3533=VECTOR('',#11884,10.);
#3534=VECTOR('',#11885,10.);
#3535=VECTOR('',#11886,10.);
#3536=VECTOR('',#11887,10.);
#3537=VECTOR('',#11890,10.);
#3538=VECTOR('',#11895,10.);
#3539=VECTOR('',#11904,10.);
#3540=VECTOR('',#11907,10.);
#3541=VECTOR('',#11910,10.);
#3542=VECTOR('',#11911,10.);
#3543=VECTOR('',#11916,10.);
#3544=VECTOR('',#11921,10.);
#3545=VECTOR('',#11928,10.);
#3546=VECTOR('',#11937,5.025);
#3547=VECTOR('',#11946,9.75);
#3548=VECTOR('',#11951,2.);
#3549=VECTOR('',#11956,2.);
#3550=VECTOR('',#11959,2.);
#3551=VECTOR('',#11962,2.);
#3552=VECTOR('',#11965,2.);
#3553=VECTOR('',#11968,1.5555);
#3554=VECTOR('',#11973,1.5555);
#3555=VECTOR('',#11978,1.5555);
#3556=VECTOR('',#11981,1.5555);
#3557=VECTOR('',#11984,1.5555);
#3558=VECTOR('',#12003,10.);
#3559=VECTOR('',#12004,10.);
#3560=VECTOR('',#12005,10.);
#3561=VECTOR('',#12006,10.);
#3562=VECTOR('',#12009,10.);
#3563=VECTOR('',#12010,10.);
#3564=VECTOR('',#12011,10.);
#3565=VECTOR('',#12014,10.);
#3566=VECTOR('',#12015,10.);
#3567=VECTOR('',#12016,10.);
#3568=VECTOR('',#12019,10.);
#3569=VECTOR('',#12020,10.);
#3570=VECTOR('',#12021,10.);
#3571=VECTOR('',#12024,10.);
#3572=VECTOR('',#12025,10.);
#3573=VECTOR('',#12026,10.);
#3574=VECTOR('',#12029,10.);
#3575=VECTOR('',#12030,10.);
#3576=VECTOR('',#12039,1.75);
#3577=VECTOR('',#12048,1.85);
#3578=VECTOR('',#12055,1.5);
#3579=VECTOR('',#12060,1.5);
#3580=VECTOR('',#12063,1.5);
#3581=VECTOR('',#12066,1.5);
#3582=VECTOR('',#12069,1.5);
#3583=VECTOR('',#12072,1.5);
#3584=VECTOR('',#12075,1.5);
#3585=VECTOR('',#12078,1.5);
#3586=VECTOR('',#12081,1.5);
#3587=VECTOR('',#12084,1.5);
#3588=VECTOR('',#12087,1.5);
#3589=VECTOR('',#12090,1.5);
#3590=VECTOR('',#12093,1.17775);
#3591=VECTOR('',#12098,1.17775);
#3592=VECTOR('',#12101,1.17775);
#3593=VECTOR('',#12104,1.17775);
#3594=VECTOR('',#12107,1.17775);
#3595=VECTOR('',#12110,1.17775);
#3596=VECTOR('',#12113,1.17775);
#3597=VECTOR('',#12116,1.17775);
#3598=VECTOR('',#12119,1.17775);
#3599=VECTOR('',#12122,1.17775);
#3600=VECTOR('',#12125,1.17775);
#3601=VECTOR('',#12128,1.17775);
#3602=VECTOR('',#12147,0.5);
#3603=VECTOR('',#12152,10.);
#3604=VECTOR('',#12153,10.);
#3605=VECTOR('',#12154,10.);
#3606=VECTOR('',#12155,10.);
#3607=VECTOR('',#12158,10.);
#3608=VECTOR('',#12159,10.);
#3609=VECTOR('',#12160,10.);
#3610=VECTOR('',#12163,10.);
#3611=VECTOR('',#12164,10.);
#3612=VECTOR('',#12165,10.);
#3613=VECTOR('',#12168,10.);
#3614=VECTOR('',#12169,10.);
#3615=VECTOR('',#12170,10.);
#3616=VECTOR('',#12173,10.);
#3617=VECTOR('',#12174,10.);
#3618=VECTOR('',#12175,10.);
#3619=VECTOR('',#12178,10.);
#3620=VECTOR('',#12179,10.);
#3621=VECTOR('',#12188,1.35);
#3622=VECTOR('',#12197,2.325);
#3623=VECTOR('',#12210,2.25);
#3624=VECTOR('',#12215,2.5);
#3625=VECTOR('',#12220,2.25);
#3626=VERTEX_POINT('',#12274);
#3627=VERTEX_POINT('',#12275);
#3628=VERTEX_POINT('',#12277);
#3629=VERTEX_POINT('',#12281);
#3630=VERTEX_POINT('',#12282);
#3631=VERTEX_POINT('',#12284);
#3632=VERTEX_POINT('',#12288);
#3633=VERTEX_POINT('',#12289);
#3634=VERTEX_POINT('',#12291);
#3635=VERTEX_POINT('',#12295);
#3636=VERTEX_POINT('',#12296);
#3637=VERTEX_POINT('',#12298);
#3638=VERTEX_POINT('',#12302);
#3639=VERTEX_POINT('',#12303);
#3640=VERTEX_POINT('',#12317);
#3641=VERTEX_POINT('',#12318);
#3642=VERTEX_POINT('',#12323);
#3643=VERTEX_POINT('',#12324);
#3644=VERTEX_POINT('',#12332);
#3645=VERTEX_POINT('',#12333);
#3646=VERTEX_POINT('',#12339);
#3647=VERTEX_POINT('',#12341);
#3648=VERTEX_POINT('',#12343);
#3649=VERTEX_POINT('',#12349);
#3650=VERTEX_POINT('',#12353);
#3651=VERTEX_POINT('',#12357);
#3652=VERTEX_POINT('',#12367);
#3653=VERTEX_POINT('',#12368);
#3654=VERTEX_POINT('',#12370);
#3655=VERTEX_POINT('',#12374);
#3656=VERTEX_POINT('',#12375);
#3657=VERTEX_POINT('',#12377);
#3658=VERTEX_POINT('',#12381);
#3659=VERTEX_POINT('',#12382);
#3660=VERTEX_POINT('',#12390);
#3661=VERTEX_POINT('',#12391);
#3662=VERTEX_POINT('',#12393);
#3663=VERTEX_POINT('',#12397);
#3664=VERTEX_POINT('',#12398);
#3665=VERTEX_POINT('',#12400);
#3666=VERTEX_POINT('',#12404);
#3667=VERTEX_POINT('',#12405);
#3668=VERTEX_POINT('',#12419);
#3669=VERTEX_POINT('',#12420);
#3670=VERTEX_POINT('',#12425);
#3671=VERTEX_POINT('',#12426);
#3672=VERTEX_POINT('',#12442);
#3673=VERTEX_POINT('',#12443);
#3674=VERTEX_POINT('',#12445);
#3675=VERTEX_POINT('',#12447);
#3676=VERTEX_POINT('',#12451);
#3677=VERTEX_POINT('',#12453);
#3678=VERTEX_POINT('',#12457);
#3679=VERTEX_POINT('',#12458);
#3680=VERTEX_POINT('',#12463);
#3681=VERTEX_POINT('',#12465);
#3682=VERTEX_POINT('',#12469);
#3683=VERTEX_POINT('',#12470);
#3684=VERTEX_POINT('',#12475);
#3685=VERTEX_POINT('',#12477);
#3686=VERTEX_POINT('',#12481);
#3687=VERTEX_POINT('',#12482);
#3688=VERTEX_POINT('',#12490);
#3689=VERTEX_POINT('',#12492);
#3690=VERTEX_POINT('',#12496);
#3691=VERTEX_POINT('',#12500);
#3692=VERTEX_POINT('',#12504);
#3693=VERTEX_POINT('',#12508);
#3694=VERTEX_POINT('',#12510);
#3695=VERTEX_POINT('',#12512);
#3696=VERTEX_POINT('',#12514);
#3697=VERTEX_POINT('',#12516);
#3698=VERTEX_POINT('',#12519);
#3699=VERTEX_POINT('',#12521);
#3700=VERTEX_POINT('',#12523);
#3701=VERTEX_POINT('',#12527);
#3702=VERTEX_POINT('',#12531);
#3703=VERTEX_POINT('',#12535);
#3704=VERTEX_POINT('',#12539);
#3705=VERTEX_POINT('',#12543);
#3706=VERTEX_POINT('',#12544);
#3707=VERTEX_POINT('',#12549);
#3708=VERTEX_POINT('',#12550);
#3709=VERTEX_POINT('',#12556);
#3710=VERTEX_POINT('',#12558);
#3711=VERTEX_POINT('',#12560);
#3712=VERTEX_POINT('',#12562);
#3713=VERTEX_POINT('',#12574);
#3714=VERTEX_POINT('',#12576);
#3715=VERTEX_POINT('',#12580);
#3716=VERTEX_POINT('',#12584);
#3717=VERTEX_POINT('',#12588);
#3718=VERTEX_POINT('',#12590);
#3719=VERTEX_POINT('',#12592);
#3720=VERTEX_POINT('',#12594);
#3721=VERTEX_POINT('',#12596);
#3722=VERTEX_POINT('',#12598);
#3723=VERTEX_POINT('',#12600);
#3724=VERTEX_POINT('',#12602);
#3725=VERTEX_POINT('',#12604);
#3726=VERTEX_POINT('',#12606);
#3727=VERTEX_POINT('',#12608);
#3728=VERTEX_POINT('',#12624);
#3729=VERTEX_POINT('',#12632);
#3730=VERTEX_POINT('',#12652);
#3731=VERTEX_POINT('',#12657);
#3732=VERTEX_POINT('',#12661);
#3733=VERTEX_POINT('',#12663);
#3734=VERTEX_POINT('',#12675);
#3735=VERTEX_POINT('',#12688);
#3736=VERTEX_POINT('',#12690);
#3737=VERTEX_POINT('',#12692);
#3738=VERTEX_POINT('',#12694);
#3739=VERTEX_POINT('',#12698);
#3740=VERTEX_POINT('',#12709);
#3741=VERTEX_POINT('',#12716);
#3742=VERTEX_POINT('',#12720);
#3743=VERTEX_POINT('',#12722);
#3744=VERTEX_POINT('',#12724);
#3745=VERTEX_POINT('',#12728);
#3746=VERTEX_POINT('',#12732);
#3747=VERTEX_POINT('',#12734);
#3748=VERTEX_POINT('',#12736);
#3749=VERTEX_POINT('',#12738);
#3750=VERTEX_POINT('',#12742);
#3751=VERTEX_POINT('',#12753);
#3752=VERTEX_POINT('',#12762);
#3753=VERTEX_POINT('',#12764);
#3754=VERTEX_POINT('',#12770);
#3755=VERTEX_POINT('',#12774);
#3756=VERTEX_POINT('',#12776);
#3757=VERTEX_POINT('',#12778);
#3758=VERTEX_POINT('',#12782);
#3759=VERTEX_POINT('',#12784);
#3760=VERTEX_POINT('',#12788);
#3761=VERTEX_POINT('',#12803);
#3762=VERTEX_POINT('',#12808);
#3763=VERTEX_POINT('',#12812);
#3764=VERTEX_POINT('',#12816);
#3765=VERTEX_POINT('',#12820);
#3766=VERTEX_POINT('',#12824);
#3767=VERTEX_POINT('',#12828);
#3768=VERTEX_POINT('',#12835);
#3769=VERTEX_POINT('',#12837);
#3770=VERTEX_POINT('',#12839);
#3771=VERTEX_POINT('',#12841);
#3772=VERTEX_POINT('',#12843);
#3773=VERTEX_POINT('',#12845);
#3774=VERTEX_POINT('',#12847);
#3775=VERTEX_POINT('',#12849);
#3776=VERTEX_POINT('',#12851);
#3777=VERTEX_POINT('',#12853);
#3778=VERTEX_POINT('',#12855);
#3779=VERTEX_POINT('',#12857);
#3780=VERTEX_POINT('',#12859);
#3781=VERTEX_POINT('',#12861);
#3782=VERTEX_POINT('',#12864);
#3783=VERTEX_POINT('',#12865);
#3784=VERTEX_POINT('',#12867);
#3785=VERTEX_POINT('',#12869);
#3786=VERTEX_POINT('',#12871);
#3787=VERTEX_POINT('',#12873);
#3788=VERTEX_POINT('',#12875);
#3789=VERTEX_POINT('',#12877);
#3790=VERTEX_POINT('',#12879);
#3791=VERTEX_POINT('',#12881);
#3792=VERTEX_POINT('',#12884);
#3793=VERTEX_POINT('',#12885);
#3794=VERTEX_POINT('',#12887);
#3795=VERTEX_POINT('',#12889);
#3796=VERTEX_POINT('',#12891);
#3797=VERTEX_POINT('',#12893);
#3798=VERTEX_POINT('',#12895);
#3799=VERTEX_POINT('',#12897);
#3800=VERTEX_POINT('',#12899);
#3801=VERTEX_POINT('',#12901);
#3802=VERTEX_POINT('',#12904);
#3803=VERTEX_POINT('',#12905);
#3804=VERTEX_POINT('',#12909);
#3805=VERTEX_POINT('',#12913);
#3806=VERTEX_POINT('',#12917);
#3807=VERTEX_POINT('',#12921);
#3808=VERTEX_POINT('',#12925);
#3809=VERTEX_POINT('',#12929);
#3810=VERTEX_POINT('',#12933);
#3811=VERTEX_POINT('',#12937);
#3812=VERTEX_POINT('',#12941);
#3813=VERTEX_POINT('',#12948);
#3814=VERTEX_POINT('',#12949);
#3815=VERTEX_POINT('',#12951);
#3816=VERTEX_POINT('',#12953);
#3817=VERTEX_POINT('',#12955);
#3818=VERTEX_POINT('',#12957);
#3819=VERTEX_POINT('',#12959);
#3820=VERTEX_POINT('',#12961);
#3821=VERTEX_POINT('',#12963);
#3822=VERTEX_POINT('',#12965);
#3823=VERTEX_POINT('',#12968);
#3824=VERTEX_POINT('',#12969);
#3825=VERTEX_POINT('',#12973);
#3826=VERTEX_POINT('',#12977);
#3827=VERTEX_POINT('',#12981);
#3828=VERTEX_POINT('',#12985);
#3829=VERTEX_POINT('',#12989);
#3830=VERTEX_POINT('',#12993);
#3831=VERTEX_POINT('',#12997);
#3832=VERTEX_POINT('',#13001);
#3833=VERTEX_POINT('',#13005);
#3834=VERTEX_POINT('',#13012);
#3835=VERTEX_POINT('',#13014);
#3836=VERTEX_POINT('',#13015);
#3837=VERTEX_POINT('',#13019);
#3838=VERTEX_POINT('',#13023);
#3839=VERTEX_POINT('',#13027);
#3840=VERTEX_POINT('',#13031);
#3841=VERTEX_POINT('',#13035);
#3842=VERTEX_POINT('',#13039);
#3843=VERTEX_POINT('',#13043);
#3844=VERTEX_POINT('',#13047);
#3845=VERTEX_POINT('',#13051);
#3846=VERTEX_POINT('',#13058);
#3847=VERTEX_POINT('',#13059);
#3848=VERTEX_POINT('',#13061);
#3849=VERTEX_POINT('',#13063);
#3850=VERTEX_POINT('',#13065);
#3851=VERTEX_POINT('',#13067);
#3852=VERTEX_POINT('',#13069);
#3853=VERTEX_POINT('',#13071);
#3854=VERTEX_POINT('',#13073);
#3855=VERTEX_POINT('',#13075);
#3856=VERTEX_POINT('',#13079);
#3857=VERTEX_POINT('',#13083);
#3858=VERTEX_POINT('',#13085);
#3859=VERTEX_POINT('',#13087);
#3860=VERTEX_POINT('',#13105);
#3861=VERTEX_POINT('',#13110);
#3862=VERTEX_POINT('',#13112);
#3863=VERTEX_POINT('',#13116);
#3864=VERTEX_POINT('',#13120);
#3865=VERTEX_POINT('',#13127);
#3866=VERTEX_POINT('',#13140);
#3867=VERTEX_POINT('',#13144);
#3868=VERTEX_POINT('',#13148);
#3869=VERTEX_POINT('',#13152);
#3870=VERTEX_POINT('',#13156);
#3871=VERTEX_POINT('',#13160);
#3872=VERTEX_POINT('',#13164);
#3873=VERTEX_POINT('',#13172);
#3874=VERTEX_POINT('',#13176);
#3875=VERTEX_POINT('',#13180);
#3876=VERTEX_POINT('',#13184);
#3877=VERTEX_POINT('',#13188);
#3878=VERTEX_POINT('',#13192);
#3879=VERTEX_POINT('',#13199);
#3880=VERTEX_POINT('',#13203);
#3881=VERTEX_POINT('',#13207);
#3882=VERTEX_POINT('',#13211);
#3883=VERTEX_POINT('',#13215);
#3884=VERTEX_POINT('',#13219);
#3885=VERTEX_POINT('',#13275);
#3886=VERTEX_POINT('',#13277);
#3887=VERTEX_POINT('',#13281);
#3888=VERTEX_POINT('',#13285);
#3889=VERTEX_POINT('',#13289);
#3890=VERTEX_POINT('',#13293);
#3891=VERTEX_POINT('',#13297);
#3892=VERTEX_POINT('',#13301);
#3893=VERTEX_POINT('',#13305);
#3894=VERTEX_POINT('',#13309);
#3895=VERTEX_POINT('',#13316);
#3896=VERTEX_POINT('',#13318);
#3897=VERTEX_POINT('',#13322);
#3898=VERTEX_POINT('',#13326);
#3899=VERTEX_POINT('',#13330);
#3900=VERTEX_POINT('',#13334);
#3901=VERTEX_POINT('',#13338);
#3902=VERTEX_POINT('',#13342);
#3903=VERTEX_POINT('',#13346);
#3904=VERTEX_POINT('',#13350);
#3905=VERTEX_POINT('',#13362);
#3906=VERTEX_POINT('',#13364);
#3907=VERTEX_POINT('',#13375);
#3908=VERTEX_POINT('',#13386);
#3909=VERTEX_POINT('',#13397);
#3910=VERTEX_POINT('',#13408);
#3911=VERTEX_POINT('',#13419);
#3912=VERTEX_POINT('',#13430);
#3913=VERTEX_POINT('',#13441);
#3914=VERTEX_POINT('',#13452);
#3915=VERTEX_POINT('',#13463);
#3916=VERTEX_POINT('',#13479);
#3917=VERTEX_POINT('',#13481);
#3918=VERTEX_POINT('',#13485);
#3919=VERTEX_POINT('',#13489);
#3920=VERTEX_POINT('',#13493);
#3921=VERTEX_POINT('',#13497);
#3922=VERTEX_POINT('',#13501);
#3923=VERTEX_POINT('',#13505);
#3924=VERTEX_POINT('',#13509);
#3925=VERTEX_POINT('',#13513);
#3926=VERTEX_POINT('',#13525);
#3927=VERTEX_POINT('',#13527);
#3928=VERTEX_POINT('',#13538);
#3929=VERTEX_POINT('',#13549);
#3930=VERTEX_POINT('',#13560);
#3931=VERTEX_POINT('',#13571);
#3932=VERTEX_POINT('',#13582);
#3933=VERTEX_POINT('',#13593);
#3934=VERTEX_POINT('',#13604);
#3935=VERTEX_POINT('',#13615);
#3936=VERTEX_POINT('',#13626);
#3937=VERTEX_POINT('',#13642);
#3938=VERTEX_POINT('',#13644);
#3939=VERTEX_POINT('',#13648);
#3940=VERTEX_POINT('',#13652);
#3941=VERTEX_POINT('',#13656);
#3942=VERTEX_POINT('',#13660);
#3943=VERTEX_POINT('',#13664);
#3944=VERTEX_POINT('',#13668);
#3945=VERTEX_POINT('',#13672);
#3946=VERTEX_POINT('',#13676);
#3947=VERTEX_POINT('',#13688);
#3948=VERTEX_POINT('',#13690);
#3949=VERTEX_POINT('',#13701);
#3950=VERTEX_POINT('',#13712);
#3951=VERTEX_POINT('',#13723);
#3952=VERTEX_POINT('',#13734);
#3953=VERTEX_POINT('',#13745);
#3954=VERTEX_POINT('',#13756);
#3955=VERTEX_POINT('',#13767);
#3956=VERTEX_POINT('',#13778);
#3957=VERTEX_POINT('',#13789);
#3958=VERTEX_POINT('',#13821);
#3959=VERTEX_POINT('',#13822);
#3960=VERTEX_POINT('',#13824);
#3961=VERTEX_POINT('',#13826);
#3962=VERTEX_POINT('',#13830);
#3963=VERTEX_POINT('',#13831);
#3964=VERTEX_POINT('',#13836);
#3965=VERTEX_POINT('',#13837);
#3966=VERTEX_POINT('',#13842);
#3967=VERTEX_POINT('',#13843);
#3968=VERTEX_POINT('',#13848);
#3969=VERTEX_POINT('',#13849);
#3970=VERTEX_POINT('',#13854);
#3971=VERTEX_POINT('',#13855);
#3972=VERTEX_POINT('',#13860);
#3973=VERTEX_POINT('',#13861);
#3974=VERTEX_POINT('',#13869);
#3975=VERTEX_POINT('',#13871);
#3976=VERTEX_POINT('',#13875);
#3977=VERTEX_POINT('',#13879);
#3978=VERTEX_POINT('',#13883);
#3979=VERTEX_POINT('',#13887);
#3980=VERTEX_POINT('',#13889);
#3981=VERTEX_POINT('',#13891);
#3982=VERTEX_POINT('',#13893);
#3983=VERTEX_POINT('',#13895);
#3984=VERTEX_POINT('',#13898);
#3985=VERTEX_POINT('',#13900);
#3986=VERTEX_POINT('',#13904);
#3987=VERTEX_POINT('',#13905);
#3988=VERTEX_POINT('',#13907);
#3989=VERTEX_POINT('',#13909);
#3990=VERTEX_POINT('',#13911);
#3991=VERTEX_POINT('',#13913);
#3992=VERTEX_POINT('',#13915);
#3993=VERTEX_POINT('',#13917);
#3994=VERTEX_POINT('',#13920);
#3995=VERTEX_POINT('',#13922);
#3996=VERTEX_POINT('',#13924);
#3997=VERTEX_POINT('',#13926);
#3998=VERTEX_POINT('',#13929);
#3999=VERTEX_POINT('',#13933);
#4000=VERTEX_POINT('',#13935);
#4001=VERTEX_POINT('',#13939);
#4002=VERTEX_POINT('',#13962);
#4003=VERTEX_POINT('',#13966);
#4004=VERTEX_POINT('',#13970);
#4005=VERTEX_POINT('',#13974);
#4006=VERTEX_POINT('',#13978);
#4007=VERTEX_POINT('',#13982);
#4008=VERTEX_POINT('',#13998);
#4009=VERTEX_POINT('',#14000);
#4010=VERTEX_POINT('',#14004);
#4011=VERTEX_POINT('',#14005);
#4012=VERTEX_POINT('',#14007);
#4013=VERTEX_POINT('',#14009);
#4014=VERTEX_POINT('',#14011);
#4015=VERTEX_POINT('',#14013);
#4016=VERTEX_POINT('',#14015);
#4017=VERTEX_POINT('',#14017);
#4018=VERTEX_POINT('',#14019);
#4019=VERTEX_POINT('',#14021);
#4020=VERTEX_POINT('',#14023);
#4021=VERTEX_POINT('',#14025);
#4022=VERTEX_POINT('',#14027);
#4023=VERTEX_POINT('',#14029);
#4024=VERTEX_POINT('',#14031);
#4025=VERTEX_POINT('',#14033);
#4026=VERTEX_POINT('',#14035);
#4027=VERTEX_POINT('',#14037);
#4028=VERTEX_POINT('',#14039);
#4029=VERTEX_POINT('',#14041);
#4030=VERTEX_POINT('',#14043);
#4031=VERTEX_POINT('',#14045);
#4032=VERTEX_POINT('',#14047);
#4033=VERTEX_POINT('',#14049);
#4034=VERTEX_POINT('',#14052);
#4035=VERTEX_POINT('',#14055);
#4036=VERTEX_POINT('',#14059);
#4037=VERTEX_POINT('',#14063);
#4038=VERTEX_POINT('',#14067);
#4039=VERTEX_POINT('',#14068);
#4040=VERTEX_POINT('',#14070);
#4041=VERTEX_POINT('',#14072);
#4042=VERTEX_POINT('',#14074);
#4043=VERTEX_POINT('',#14076);
#4044=VERTEX_POINT('',#14080);
#4045=VERTEX_POINT('',#14082);
#4046=VERTEX_POINT('',#14086);
#4047=VERTEX_POINT('',#14088);
#4048=VERTEX_POINT('',#14090);
#4049=VERTEX_POINT('',#14094);
#4050=VERTEX_POINT('',#14096);
#4051=VERTEX_POINT('',#14100);
#4052=VERTEX_POINT('',#14102);
#4053=VERTEX_POINT('',#14104);
#4054=VERTEX_POINT('',#14111);
#4055=VERTEX_POINT('',#14115);
#4056=VERTEX_POINT('',#14117);
#4057=VERTEX_POINT('',#14121);
#4058=VERTEX_POINT('',#14123);
#4059=VERTEX_POINT('',#14125);
#4060=VERTEX_POINT('',#14127);
#4061=VERTEX_POINT('',#14129);
#4062=VERTEX_POINT('',#14131);
#4063=VERTEX_POINT('',#14133);
#4064=VERTEX_POINT('',#14135);
#4065=VERTEX_POINT('',#14137);
#4066=VERTEX_POINT('',#14139);
#4067=VERTEX_POINT('',#14141);
#4068=VERTEX_POINT('',#14143);
#4069=VERTEX_POINT('',#14145);
#4070=VERTEX_POINT('',#14147);
#4071=VERTEX_POINT('',#14149);
#4072=VERTEX_POINT('',#14151);
#4073=VERTEX_POINT('',#14153);
#4074=VERTEX_POINT('',#14155);
#4075=VERTEX_POINT('',#14157);
#4076=VERTEX_POINT('',#14159);
#4077=VERTEX_POINT('',#14161);
#4078=VERTEX_POINT('',#14164);
#4079=VERTEX_POINT('',#14167);
#4080=VERTEX_POINT('',#14171);
#4081=VERTEX_POINT('',#14175);
#4082=VERTEX_POINT('',#14179);
#4083=VERTEX_POINT('',#14180);
#4084=VERTEX_POINT('',#14187);
#4085=VERTEX_POINT('',#14191);
#4086=VERTEX_POINT('',#14198);
#4087=VERTEX_POINT('',#14203);
#4088=VERTEX_POINT('',#14205);
#4089=VERTEX_POINT('',#14209);
#4090=VERTEX_POINT('',#14210);
#4091=VERTEX_POINT('',#14215);
#4092=VERTEX_POINT('',#14217);
#4093=VERTEX_POINT('',#14224);
#4094=VERTEX_POINT('',#14226);
#4095=VERTEX_POINT('',#14230);
#4096=VERTEX_POINT('',#14234);
#4097=VERTEX_POINT('',#14239);
#4098=VERTEX_POINT('',#14241);
#4099=VERTEX_POINT('',#14243);
#4100=VERTEX_POINT('',#14248);
#4101=VERTEX_POINT('',#14252);
#4102=VERTEX_POINT('',#14253);
#4103=VERTEX_POINT('',#14258);
#4104=VERTEX_POINT('',#14262);
#4105=VERTEX_POINT('',#14266);
#4106=VERTEX_POINT('',#14270);
#4107=VERTEX_POINT('',#14274);
#4108=VERTEX_POINT('',#14280);
#4109=VERTEX_POINT('',#14284);
#4110=VERTEX_POINT('',#14288);
#4111=VERTEX_POINT('',#14292);
#4112=VERTEX_POINT('',#14296);
#4113=VERTEX_POINT('',#14300);
#4114=VERTEX_POINT('',#14304);
#4115=VERTEX_POINT('',#14308);
#4116=VERTEX_POINT('',#14312);
#4117=VERTEX_POINT('',#14318);
#4118=VERTEX_POINT('',#14320);
#4119=VERTEX_POINT('',#14324);
#4120=VERTEX_POINT('',#14328);
#4121=VERTEX_POINT('',#14332);
#4122=VERTEX_POINT('',#14336);
#4123=VERTEX_POINT('',#14340);
#4124=VERTEX_POINT('',#14362);
#4125=VERTEX_POINT('',#14366);
#4126=VERTEX_POINT('',#14370);
#4127=VERTEX_POINT('',#14374);
#4128=VERTEX_POINT('',#14378);
#4129=VERTEX_POINT('',#14382);
#4130=VERTEX_POINT('',#14384);
#4131=VERTEX_POINT('',#14388);
#4132=VERTEX_POINT('',#14392);
#4133=VERTEX_POINT('',#14405);
#4134=VERTEX_POINT('',#14407);
#4135=VERTEX_POINT('',#14409);
#4136=VERTEX_POINT('',#14439);
#4137=VERTEX_POINT('',#14442);
#4138=VERTEX_POINT('',#14446);
#4139=VERTEX_POINT('',#14450);
#4140=VERTEX_POINT('',#14456);
#4141=VERTEX_POINT('',#14458);
#4142=VERTEX_POINT('',#14460);
#4143=VERTEX_POINT('',#14464);
#4144=VERTEX_POINT('',#14469);
#4145=VERTEX_POINT('',#14470);
#4146=VERTEX_POINT('',#14474);
#4147=VERTEX_POINT('',#14476);
#4148=VERTEX_POINT('',#14483);
#4149=VERTEX_POINT('',#14488);
#4150=VERTEX_POINT('',#14489);
#4151=VERTEX_POINT('',#14496);
#4152=VERTEX_POINT('',#14500);
#4153=VERTEX_POINT('',#14506);
#4154=VERTEX_POINT('',#14507);
#4155=VERTEX_POINT('',#14510);
#4156=VERTEX_POINT('',#14515);
#4157=VERTEX_POINT('',#14519);
#4158=VERTEX_POINT('',#14523);
#4159=VERTEX_POINT('',#14526);
#4160=VERTEX_POINT('',#14530);
#4161=VERTEX_POINT('',#14536);
#4162=VERTEX_POINT('',#14537);
#4163=VERTEX_POINT('',#14540);
#4164=VERTEX_POINT('',#14544);
#4165=VERTEX_POINT('',#14547);
#4166=VERTEX_POINT('',#14551);
#4167=VERTEX_POINT('',#14555);
#4168=VERTEX_POINT('',#14558);
#4169=VERTEX_POINT('',#14564);
#4170=VERTEX_POINT('',#14565);
#4171=VERTEX_POINT('',#14567);
#4172=VERTEX_POINT('',#14569);
#4173=VERTEX_POINT('',#14573);
#4174=VERTEX_POINT('',#14575);
#4175=VERTEX_POINT('',#14579);
#4176=VERTEX_POINT('',#14581);
#4177=VERTEX_POINT('',#14583);
#4178=VERTEX_POINT('',#14587);
#4179=VERTEX_POINT('',#14589);
#4180=VERTEX_POINT('',#14595);
#4181=VERTEX_POINT('',#14596);
#4182=VERTEX_POINT('',#14598);
#4183=VERTEX_POINT('',#14600);
#4184=VERTEX_POINT('',#14604);
#4185=VERTEX_POINT('',#14606);
#4186=VERTEX_POINT('',#14610);
#4187=VERTEX_POINT('',#14612);
#4188=VERTEX_POINT('',#14614);
#4189=VERTEX_POINT('',#14618);
#4190=VERTEX_POINT('',#14622);
#4191=VERTEX_POINT('',#14705);
#4192=VERTEX_POINT('',#14706);
#4193=VERTEX_POINT('',#14749);
#4194=VERTEX_POINT('',#14751);
#4195=VERTEX_POINT('',#14789);
#4196=VERTEX_POINT('',#14791);
#4197=VERTEX_POINT('',#14793);
#4198=VERTEX_POINT('',#14795);
#4199=VERTEX_POINT('',#14797);
#4200=VERTEX_POINT('',#14800);
#4201=VERTEX_POINT('',#14803);
#4202=VERTEX_POINT('',#14805);
#4203=VERTEX_POINT('',#14809);
#4204=VERTEX_POINT('',#14812);
#4205=VERTEX_POINT('',#14813);
#4206=VERTEX_POINT('',#14817);
#4207=VERTEX_POINT('',#14819);
#4208=VERTEX_POINT('',#14825);
#4209=VERTEX_POINT('',#14829);
#4210=VERTEX_POINT('',#14835);
#4211=VERTEX_POINT('',#14836);
#4212=VERTEX_POINT('',#14838);
#4213=VERTEX_POINT('',#14840);
#4214=VERTEX_POINT('',#14844);
#4215=VERTEX_POINT('',#14846);
#4216=VERTEX_POINT('',#14850);
#4217=VERTEX_POINT('',#14851);
#4218=VERTEX_POINT('',#14853);
#4219=VERTEX_POINT('',#14855);
#4220=VERTEX_POINT('',#14859);
#4221=VERTEX_POINT('',#14861);
#4222=VERTEX_POINT('',#14865);
#4223=VERTEX_POINT('',#14866);
#4224=VERTEX_POINT('',#14868);
#4225=VERTEX_POINT('',#14870);
#4226=VERTEX_POINT('',#14874);
#4227=VERTEX_POINT('',#14876);
#4228=VERTEX_POINT('',#14880);
#4229=VERTEX_POINT('',#14881);
#4230=VERTEX_POINT('',#14883);
#4231=VERTEX_POINT('',#14885);
#4232=VERTEX_POINT('',#14889);
#4233=VERTEX_POINT('',#14891);
#4234=VERTEX_POINT('',#14895);
#4235=VERTEX_POINT('',#14896);
#4236=VERTEX_POINT('',#14900);
#4237=VERTEX_POINT('',#14902);
#4238=VERTEX_POINT('',#14908);
#4239=VERTEX_POINT('',#14912);
#4240=VERTEX_POINT('',#14918);
#4241=VERTEX_POINT('',#14919);
#4242=VERTEX_POINT('',#14923);
#4243=VERTEX_POINT('',#14925);
#4244=VERTEX_POINT('',#14931);
#4245=VERTEX_POINT('',#14935);
#4246=VERTEX_POINT('',#14941);
#4247=VERTEX_POINT('',#14942);
#4248=VERTEX_POINT('',#14944);
#4249=VERTEX_POINT('',#14946);
#4250=VERTEX_POINT('',#14950);
#4251=VERTEX_POINT('',#14952);
#4252=VERTEX_POINT('',#14956);
#4253=VERTEX_POINT('',#14957);
#4254=VERTEX_POINT('',#14959);
#4255=VERTEX_POINT('',#14961);
#4256=VERTEX_POINT('',#14965);
#4257=VERTEX_POINT('',#14967);
#4258=VERTEX_POINT('',#14971);
#4259=VERTEX_POINT('',#14972);
#4260=VERTEX_POINT('',#14976);
#4261=VERTEX_POINT('',#14978);
#4262=VERTEX_POINT('',#14984);
#4263=VERTEX_POINT('',#14988);
#4264=VERTEX_POINT('',#14994);
#4265=VERTEX_POINT('',#14995);
#4266=VERTEX_POINT('',#14997);
#4267=VERTEX_POINT('',#14999);
#4268=VERTEX_POINT('',#15003);
#4269=VERTEX_POINT('',#15005);
#4270=VERTEX_POINT('',#15009);
#4271=VERTEX_POINT('',#15010);
#4272=VERTEX_POINT('',#15014);
#4273=VERTEX_POINT('',#15016);
#4274=VERTEX_POINT('',#15022);
#4275=VERTEX_POINT('',#15026);
#4276=VERTEX_POINT('',#15032);
#4277=VERTEX_POINT('',#15033);
#4278=VERTEX_POINT('',#15037);
#4279=VERTEX_POINT('',#15039);
#4280=VERTEX_POINT('',#15045);
#4281=VERTEX_POINT('',#15049);
#4282=VERTEX_POINT('',#15055);
#4283=VERTEX_POINT('',#15057);
#4284=VERTEX_POINT('',#15059);
#4285=VERTEX_POINT('',#15065);
#4286=VERTEX_POINT('',#15067);
#4287=VERTEX_POINT('',#15081);
#4288=VERTEX_POINT('',#15094);
#4289=VERTEX_POINT('',#15106);
#4290=VERTEX_POINT('',#15115);
#4291=VERTEX_POINT('',#15125);
#4292=VERTEX_POINT('',#15132);
#4293=VERTEX_POINT('',#15137);
#4294=VERTEX_POINT('',#15159);
#4295=VERTEX_POINT('',#15163);
#4296=VERTEX_POINT('',#15169);
#4297=VERTEX_POINT('',#15170);
#4298=VERTEX_POINT('',#15172);
#4299=VERTEX_POINT('',#15183);
#4300=VERTEX_POINT('',#15193);
#4301=VERTEX_POINT('',#15194);
#4302=VERTEX_POINT('',#15241);
#4303=VERTEX_POINT('',#15242);
#4304=VERTEX_POINT('',#15289);
#4305=VERTEX_POINT('',#15290);
#4306=VERTEX_POINT('',#15343);
#4307=VERTEX_POINT('',#15344);
#4308=VERTEX_POINT('',#15391);
#4309=VERTEX_POINT('',#15392);
#4310=VERTEX_POINT('',#15394);
#4311=VERTEX_POINT('',#15401);
#4312=VERTEX_POINT('',#15402);
#4313=VERTEX_POINT('',#15414);
#4314=VERTEX_POINT('',#15426);
#4315=VERTEX_POINT('',#15427);
#4316=VERTEX_POINT('',#15451);
#4317=VERTEX_POINT('',#15452);
#4318=VERTEX_POINT('',#15476);
#4319=VERTEX_POINT('',#15477);
#4320=VERTEX_POINT('',#15500);
#4321=VERTEX_POINT('',#15589);
#4322=VERTEX_POINT('',#15591);
#4323=VERTEX_POINT('',#15834);
#4324=VERTEX_POINT('',#15933);
#4325=VERTEX_POINT('',#15936);
#4326=VERTEX_POINT('',#16186);
#4327=VERTEX_POINT('',#16187);
#4328=VERTEX_POINT('',#16189);
#4329=VERTEX_POINT('',#16191);
#4330=VERTEX_POINT('',#16195);
#4331=VERTEX_POINT('',#16197);
#4332=VERTEX_POINT('',#16201);
#4333=VERTEX_POINT('',#16203);
#4334=VERTEX_POINT('',#16207);
#4335=VERTEX_POINT('',#16209);
#4336=VERTEX_POINT('',#16213);
#4337=VERTEX_POINT('',#16215);
#4338=VERTEX_POINT('',#16223);
#4339=VERTEX_POINT('',#16230);
#4340=VERTEX_POINT('',#16236);
#4341=VERTEX_POINT('',#16237);
#4342=VERTEX_POINT('',#16239);
#4343=VERTEX_POINT('',#16250);
#4344=VERTEX_POINT('',#16260);
#4345=VERTEX_POINT('',#16261);
#4346=VERTEX_POINT('',#16308);
#4347=VERTEX_POINT('',#16309);
#4348=VERTEX_POINT('',#16356);
#4349=VERTEX_POINT('',#16357);
#4350=VERTEX_POINT('',#16410);
#4351=VERTEX_POINT('',#16411);
#4352=VERTEX_POINT('',#16458);
#4353=VERTEX_POINT('',#16459);
#4354=VERTEX_POINT('',#16506);
#4355=VERTEX_POINT('',#16507);
#4356=VERTEX_POINT('',#16560);
#4357=VERTEX_POINT('',#16561);
#4358=VERTEX_POINT('',#16608);
#4359=VERTEX_POINT('',#16609);
#4360=VERTEX_POINT('',#16656);
#4361=VERTEX_POINT('',#16657);
#4362=VERTEX_POINT('',#16710);
#4363=VERTEX_POINT('',#16711);
#4364=VERTEX_POINT('',#16758);
#4365=VERTEX_POINT('',#16759);
#4366=VERTEX_POINT('',#16812);
#4367=VERTEX_POINT('',#16813);
#4368=VERTEX_POINT('',#16815);
#4369=VERTEX_POINT('',#16822);
#4370=VERTEX_POINT('',#16830);
#4371=VERTEX_POINT('',#16831);
#4372=VERTEX_POINT('',#16855);
#4373=VERTEX_POINT('',#16856);
#4374=VERTEX_POINT('',#16880);
#4375=VERTEX_POINT('',#16881);
#4376=VERTEX_POINT('',#16905);
#4377=VERTEX_POINT('',#16906);
#4378=VERTEX_POINT('',#16930);
#4379=VERTEX_POINT('',#16931);
#4380=VERTEX_POINT('',#16954);
#4381=VERTEX_POINT('',#16955);
#4382=VERTEX_POINT('',#16979);
#4383=VERTEX_POINT('',#16980);
#4384=VERTEX_POINT('',#17004);
#4385=VERTEX_POINT('',#17005);
#4386=VERTEX_POINT('',#17028);
#4387=VERTEX_POINT('',#17029);
#4388=VERTEX_POINT('',#17053);
#4389=VERTEX_POINT('',#17054);
#4390=VERTEX_POINT('',#17078);
#4391=VERTEX_POINT('',#17079);
#4392=VERTEX_POINT('',#17102);
#4393=VERTEX_POINT('',#17188);
#4394=VERTEX_POINT('',#17190);
#4395=VERTEX_POINT('',#17621);
#4396=VERTEX_POINT('',#17717);
#4397=VERTEX_POINT('',#17720);
#4398=VERTEX_POINT('',#18158);
#4399=VERTEX_POINT('',#18159);
#4400=VERTEX_POINT('',#18163);
#4401=VERTEX_POINT('',#18164);
#4402=VERTEX_POINT('',#18166);
#4403=VERTEX_POINT('',#18168);
#4404=VERTEX_POINT('',#18172);
#4405=VERTEX_POINT('',#18174);
#4406=VERTEX_POINT('',#18178);
#4407=VERTEX_POINT('',#18180);
#4408=VERTEX_POINT('',#18184);
#4409=VERTEX_POINT('',#18186);
#4410=VERTEX_POINT('',#18190);
#4411=VERTEX_POINT('',#18192);
#4412=VERTEX_POINT('',#18200);
#4413=VERTEX_POINT('',#18207);
#4414=VERTEX_POINT('',#18213);
#4415=VERTEX_POINT('',#18216);
#4416=VERTEX_POINT('',#18220);
#4417=VERTEX_POINT('',#18224);
#4418=EDGE_CURVE('',#3626,#3627,#1936,.T.);
#4419=EDGE_CURVE('',#3628,#3626,#1937,.T.);
#4420=EDGE_CURVE('',#3627,#3628,#1938,.T.);
#4421=EDGE_CURVE('',#3629,#3630,#1939,.T.);
#4422=EDGE_CURVE('',#3631,#3629,#1940,.T.);
#4423=EDGE_CURVE('',#3630,#3631,#1941,.T.);
#4424=EDGE_CURVE('',#3632,#3633,#1942,.T.);
#4425=EDGE_CURVE('',#3634,#3632,#1943,.T.);
#4426=EDGE_CURVE('',#3633,#3634,#1944,.T.);
#4427=EDGE_CURVE('',#3635,#3636,#1945,.T.);
#4428=EDGE_CURVE('',#3637,#3635,#1946,.T.);
#4429=EDGE_CURVE('',#3636,#3637,#1947,.T.);
#4430=EDGE_CURVE('',#3638,#3639,#822,.T.);
#4431=EDGE_CURVE('',#3639,#3637,#1948,.T.);
#4432=EDGE_CURVE('',#3635,#3638,#1949,.T.);
#4433=EDGE_CURVE('',#3629,#3636,#1950,.T.);
#4434=EDGE_CURVE('',#3637,#3631,#1951,.T.);
#4435=EDGE_CURVE('',#3632,#3635,#1952,.T.);
#4436=EDGE_CURVE('',#3636,#3634,#1953,.T.);
#4437=EDGE_CURVE('',#3627,#3633,#1954,.T.);
#4438=EDGE_CURVE('',#3634,#3626,#1955,.T.);
#4439=EDGE_CURVE('',#3640,#3641,#823,.T.);
#4440=EDGE_CURVE('',#3641,#3632,#1956,.T.);
#4441=EDGE_CURVE('',#3633,#3640,#1957,.T.);
#4442=EDGE_CURVE('',#3642,#3643,#824,.T.);
#4443=EDGE_CURVE('',#3643,#3630,#1958,.T.);
#4444=EDGE_CURVE('',#3631,#3642,#1959,.T.);
#4445=EDGE_CURVE('',#3626,#3629,#1960,.T.);
#4446=EDGE_CURVE('',#3630,#3628,#1961,.T.);
#4447=EDGE_CURVE('',#3644,#3645,#825,.T.);
#4448=EDGE_CURVE('',#3645,#3627,#1962,.T.);
#4449=EDGE_CURVE('',#3628,#3644,#1963,.T.);
#4450=EDGE_CURVE('',#3641,#3638,#1964,.T.);
#4451=EDGE_CURVE('',#3646,#3646,#629,.T.);
#4452=EDGE_CURVE('',#3647,#3647,#630,.T.);
#4453=EDGE_CURVE('',#3648,#3648,#631,.T.);
#4454=EDGE_CURVE('',#3645,#3640,#632,.T.);
#4455=EDGE_CURVE('',#3649,#3649,#633,.T.);
#4456=EDGE_CURVE('',#3649,#3648,#1965,.T.);
#4457=EDGE_CURVE('',#3650,#3650,#634,.T.);
#4458=EDGE_CURVE('',#3650,#3647,#1966,.T.);
#4459=EDGE_CURVE('',#3651,#3651,#635,.T.);
#4460=EDGE_CURVE('',#3651,#3646,#1967,.T.);
#4461=EDGE_CURVE('',#3643,#3644,#1968,.T.);
#4462=EDGE_CURVE('',#3639,#3642,#636,.T.);
#4463=EDGE_CURVE('',#3652,#3653,#1969,.T.);
#4464=EDGE_CURVE('',#3654,#3652,#1970,.T.);
#4465=EDGE_CURVE('',#3653,#3654,#1971,.T.);
#4466=EDGE_CURVE('',#3655,#3656,#1972,.T.);
#4467=EDGE_CURVE('',#3657,#3655,#1973,.T.);
#4468=EDGE_CURVE('',#3656,#3657,#1974,.T.);
#4469=EDGE_CURVE('',#3658,#3659,#826,.T.);
#4470=EDGE_CURVE('',#3659,#3657,#1975,.T.);
#4471=EDGE_CURVE('',#3655,#3658,#1976,.T.);
#4472=EDGE_CURVE('',#3652,#3656,#1977,.T.);
#4473=EDGE_CURVE('',#3657,#3654,#1978,.T.);
#4474=EDGE_CURVE('',#3660,#3661,#1979,.T.);
#4475=EDGE_CURVE('',#3662,#3660,#1980,.T.);
#4476=EDGE_CURVE('',#3661,#3662,#1981,.T.);
#4477=EDGE_CURVE('',#3663,#3664,#1982,.T.);
#4478=EDGE_CURVE('',#3665,#3663,#1983,.T.);
#4479=EDGE_CURVE('',#3664,#3665,#1984,.T.);
#4480=EDGE_CURVE('',#3666,#3667,#827,.T.);
#4481=EDGE_CURVE('',#3667,#3665,#1985,.T.);
#4482=EDGE_CURVE('',#3663,#3666,#1986,.T.);
#4483=EDGE_CURVE('',#3656,#3664,#1987,.T.);
#4484=EDGE_CURVE('',#3665,#3655,#1988,.T.);
#4485=EDGE_CURVE('',#3660,#3663,#1989,.T.);
#4486=EDGE_CURVE('',#3664,#3662,#1990,.T.);
#4487=EDGE_CURVE('',#3653,#3661,#1991,.T.);
#4488=EDGE_CURVE('',#3662,#3652,#1992,.T.);
#4489=EDGE_CURVE('',#3668,#3669,#828,.T.);
#4490=EDGE_CURVE('',#3669,#3660,#1993,.T.);
#4491=EDGE_CURVE('',#3661,#3668,#1994,.T.);
#4492=EDGE_CURVE('',#3670,#3671,#829,.T.);
#4493=EDGE_CURVE('',#3671,#3653,#1995,.T.);
#4494=EDGE_CURVE('',#3654,#3670,#1996,.T.);
#4495=EDGE_CURVE('',#3669,#3666,#1997,.T.);
#4496=EDGE_CURVE('',#3671,#3668,#637,.T.);
#4497=EDGE_CURVE('',#3659,#3670,#1998,.T.);
#4498=EDGE_CURVE('',#3667,#3658,#638,.T.);
#4499=EDGE_CURVE('',#3672,#3673,#1999,.T.);
#4500=EDGE_CURVE('',#3673,#3674,#2000,.T.);
#4501=EDGE_CURVE('',#3674,#3675,#2001,.T.);
#4502=EDGE_CURVE('',#3675,#3672,#2002,.T.);
#4503=EDGE_CURVE('',#3672,#3676,#639,.T.);
#4504=EDGE_CURVE('',#3676,#3677,#2003,.T.);
#4505=EDGE_CURVE('',#3677,#3673,#640,.T.);
#4506=EDGE_CURVE('',#3678,#3679,#2004,.T.);
#4507=EDGE_CURVE('',#3679,#3677,#2005,.T.);
#4508=EDGE_CURVE('',#3676,#3678,#2006,.T.);
#4509=EDGE_CURVE('',#3678,#3680,#641,.T.);
#4510=EDGE_CURVE('',#3680,#3681,#2007,.T.);
#4511=EDGE_CURVE('',#3681,#3679,#642,.T.);
#4512=EDGE_CURVE('',#3682,#3683,#2008,.T.);
#4513=EDGE_CURVE('',#3683,#3681,#2009,.T.);
#4514=EDGE_CURVE('',#3680,#3682,#2010,.T.);
#4515=EDGE_CURVE('',#3682,#3684,#643,.T.);
#4516=EDGE_CURVE('',#3684,#3685,#2011,.T.);
#4517=EDGE_CURVE('',#3685,#3683,#644,.T.);
#4518=EDGE_CURVE('',#3686,#3687,#2012,.T.);
#4519=EDGE_CURVE('',#3687,#3685,#2013,.T.);
#4520=EDGE_CURVE('',#3684,#3686,#2014,.T.);
#4521=EDGE_CURVE('',#3686,#3675,#645,.T.);
#4522=EDGE_CURVE('',#3674,#3687,#646,.T.);
#4523=EDGE_CURVE('',#3678,#3688,#2015,.T.);
#4524=EDGE_CURVE('',#3689,#3688,#647,.T.);
#4525=EDGE_CURVE('',#3689,#3680,#2016,.T.);
#4526=EDGE_CURVE('',#3690,#3676,#2017,.T.);
#4527=EDGE_CURVE('',#3688,#3690,#2018,.T.);
#4528=EDGE_CURVE('',#3672,#3691,#2019,.T.);
#4529=EDGE_CURVE('',#3690,#3691,#648,.T.);
#4530=EDGE_CURVE('',#3692,#3675,#2020,.T.);
#4531=EDGE_CURVE('',#3691,#3692,#2021,.T.);
#4532=EDGE_CURVE('',#3693,#3693,#649,.T.);
#4533=EDGE_CURVE('',#3694,#3694,#650,.T.);
#4534=EDGE_CURVE('',#3695,#3695,#651,.T.);
#4535=EDGE_CURVE('',#3696,#3696,#652,.T.);
#4536=EDGE_CURVE('',#3697,#3697,#653,.T.);
#4537=EDGE_CURVE('',#3689,#3698,#2022,.T.);
#4538=EDGE_CURVE('',#3698,#3699,#2023,.T.);
#4539=EDGE_CURVE('',#3699,#3700,#2024,.T.);
#4540=EDGE_CURVE('',#3700,#3689,#2025,.T.);
#4541=EDGE_CURVE('',#3688,#3701,#2026,.T.);
#4542=EDGE_CURVE('',#3701,#3698,#654,.T.);
#4543=EDGE_CURVE('',#3690,#3702,#2027,.T.);
#4544=EDGE_CURVE('',#3702,#3701,#2028,.T.);
#4545=EDGE_CURVE('',#3691,#3703,#2029,.T.);
#4546=EDGE_CURVE('',#3703,#3702,#655,.T.);
#4547=EDGE_CURVE('',#3692,#3704,#2030,.T.);
#4548=EDGE_CURVE('',#3704,#3703,#2031,.T.);
#4549=EDGE_CURVE('',#3705,#3706,#2032,.T.);
#4550=EDGE_CURVE('',#3706,#3704,#656,.T.);
#4551=EDGE_CURVE('',#3692,#3705,#657,.T.);
#4552=EDGE_CURVE('',#3707,#3708,#188,.T.);
#4553=EDGE_CURVE('',#3708,#3706,#2033,.T.);
#4554=EDGE_CURVE('',#3705,#3709,#2034,.T.);
#4555=EDGE_CURVE('',#3709,#3710,#2035,.T.);
#4556=EDGE_CURVE('',#3710,#3711,#2036,.T.);
#4557=EDGE_CURVE('',#3711,#3712,#189,.T.);
#4558=EDGE_CURVE('',#3712,#3707,#2037,.T.);
#4559=EDGE_CURVE('',#3699,#3710,#658,.T.);
#4560=EDGE_CURVE('',#3709,#3700,#659,.T.);
#4561=EDGE_CURVE('',#3682,#3700,#2038,.T.);
#4562=EDGE_CURVE('',#3713,#3703,#2039,.T.);
#4563=EDGE_CURVE('',#3714,#3713,#660,.T.);
#4564=EDGE_CURVE('',#3714,#3702,#2040,.T.);
#4565=EDGE_CURVE('',#3715,#3704,#2041,.T.);
#4566=EDGE_CURVE('',#3713,#3715,#2042,.T.);
#4567=EDGE_CURVE('',#3716,#3706,#2043,.T.);
#4568=EDGE_CURVE('',#3715,#3716,#661,.T.);
#4569=EDGE_CURVE('',#3717,#3710,#2044,.T.);
#4570=EDGE_CURVE('',#3718,#3717,#2045,.T.);
#4571=EDGE_CURVE('',#3718,#3719,#2046,.T.);
#4572=EDGE_CURVE('',#3719,#3720,#2047,.T.);
#4573=EDGE_CURVE('',#3720,#3721,#2048,.T.);
#4574=EDGE_CURVE('',#3722,#3721,#2049,.T.);
#4575=EDGE_CURVE('',#3722,#3723,#2050,.T.);
#4576=EDGE_CURVE('',#3723,#3724,#2051,.T.);
#4577=EDGE_CURVE('',#3724,#3725,#2052,.T.);
#4578=EDGE_CURVE('',#3725,#3726,#2053,.T.);
#4579=EDGE_CURVE('',#3726,#3727,#190,.T.);
#4580=EDGE_CURVE('',#3711,#3727,#191,.T.);
#4581=EDGE_CURVE('',#3728,#3708,#192,.T.);
#4582=EDGE_CURVE('',#3728,#3729,#193,.T.);
#4583=EDGE_CURVE('',#3716,#3729,#2054,.T.);
#4584=EDGE_CURVE('',#3730,#3707,#194,.F.);
#4585=EDGE_CURVE('',#3730,#3731,#195,.T.);
#4586=EDGE_CURVE('',#3732,#3731,#2055,.T.);
#4587=EDGE_CURVE('',#3733,#3732,#196,.T.);
#4588=EDGE_CURVE('',#3729,#3733,#197,.T.);
#4589=EDGE_CURVE('',#3712,#3734,#198,.F.);
#4590=EDGE_CURVE('',#3734,#3730,#2056,.T.);
#4591=EDGE_CURVE('',#3735,#3735,#662,.T.);
#4592=EDGE_CURVE('',#3735,#3736,#2057,.T.);
#4593=EDGE_CURVE('',#3736,#3737,#663,.T.);
#4594=EDGE_CURVE('',#3737,#3738,#107,.T.);
#4595=EDGE_CURVE('',#3738,#3739,#199,.T.);
#4596=EDGE_CURVE('',#3739,#3740,#108,.T.);
#4597=EDGE_CURVE('',#3740,#3736,#664,.T.);
#4598=EDGE_CURVE('',#3738,#3717,#2058,.T.);
#4599=EDGE_CURVE('',#3717,#3741,#665,.T.);
#4600=EDGE_CURVE('',#3739,#3741,#2059,.T.);
#4601=EDGE_CURVE('',#3737,#3742,#2060,.T.);
#4602=EDGE_CURVE('',#3742,#3743,#2061,.T.);
#4603=EDGE_CURVE('',#3743,#3744,#2062,.T.);
#4604=EDGE_CURVE('',#3744,#3718,#2063,.T.);
#4605=EDGE_CURVE('',#3735,#3745,#2064,.T.);
#4606=EDGE_CURVE('',#3745,#3745,#666,.T.);
#4607=EDGE_CURVE('',#3746,#3746,#667,.T.);
#4608=EDGE_CURVE('',#3746,#3747,#2065,.T.);
#4609=EDGE_CURVE('',#3747,#3748,#668,.T.);
#4610=EDGE_CURVE('',#3748,#3749,#109,.T.);
#4611=EDGE_CURVE('',#3749,#3750,#200,.T.);
#4612=EDGE_CURVE('',#3750,#3751,#110,.T.);
#4613=EDGE_CURVE('',#3751,#3747,#669,.T.);
#4614=EDGE_CURVE('',#3749,#3715,#2066,.T.);
#4615=EDGE_CURVE('',#3750,#3716,#2067,.T.);
#4616=EDGE_CURVE('',#3748,#3752,#2068,.T.);
#4617=EDGE_CURVE('',#3753,#3752,#111,.T.);
#4618=EDGE_CURVE('',#3753,#3713,#2069,.T.);
#4619=EDGE_CURVE('',#3746,#3754,#2070,.T.);
#4620=EDGE_CURVE('',#3754,#3754,#670,.T.);
#4621=EDGE_CURVE('',#3755,#3755,#671,.T.);
#4622=EDGE_CURVE('',#3755,#3756,#2071,.T.);
#4623=EDGE_CURVE('',#3756,#3757,#112,.T.);
#4624=EDGE_CURVE('',#3757,#3758,#672,.T.);
#4625=EDGE_CURVE('',#3758,#3759,#113,.T.);
#4626=EDGE_CURVE('',#3759,#3760,#201,.T.);
#4627=EDGE_CURVE('',#3760,#3756,#114,.T.);
#4628=EDGE_CURVE('',#3741,#3761,#2072,.T.);
#4629=EDGE_CURVE('',#3759,#3761,#2073,.T.);
#4630=EDGE_CURVE('',#3758,#3740,#2074,.T.);
#4631=EDGE_CURVE('',#3762,#3757,#2075,.T.);
#4632=EDGE_CURVE('',#3752,#3762,#673,.T.);
#4633=EDGE_CURVE('',#3733,#3751,#2076,.T.);
#4634=EDGE_CURVE('',#3732,#3763,#202,.T.);
#4635=EDGE_CURVE('',#3763,#3764,#203,.T.);
#4636=EDGE_CURVE('',#3764,#3765,#204,.T.);
#4637=EDGE_CURVE('',#3765,#3766,#205,.T.);
#4638=EDGE_CURVE('',#3766,#3767,#206,.T.);
#4639=EDGE_CURVE('',#3767,#3726,#207,.T.);
#4640=EDGE_CURVE('',#3725,#3768,#2077,.T.);
#4641=EDGE_CURVE('',#3768,#3769,#2078,.T.);
#4642=EDGE_CURVE('',#3769,#3770,#2079,.T.);
#4643=EDGE_CURVE('',#3770,#3771,#2080,.T.);
#4644=EDGE_CURVE('',#3771,#3772,#2081,.T.);
#4645=EDGE_CURVE('',#3772,#3773,#2082,.T.);
#4646=EDGE_CURVE('',#3773,#3774,#2083,.T.);
#4647=EDGE_CURVE('',#3775,#3774,#2084,.T.);
#4648=EDGE_CURVE('',#3775,#3776,#2085,.T.);
#4649=EDGE_CURVE('',#3776,#3777,#2086,.T.);
#4650=EDGE_CURVE('',#3777,#3778,#2087,.T.);
#4651=EDGE_CURVE('',#3778,#3779,#2088,.T.);
#4652=EDGE_CURVE('',#3779,#3780,#2089,.T.);
#4653=EDGE_CURVE('',#3780,#3781,#2090,.T.);
#4654=EDGE_CURVE('',#3781,#3742,#2091,.T.);
#4655=EDGE_CURVE('',#3782,#3783,#2092,.T.);
#4656=EDGE_CURVE('',#3783,#3784,#2093,.T.);
#4657=EDGE_CURVE('',#3784,#3785,#2094,.T.);
#4658=EDGE_CURVE('',#3785,#3786,#2095,.T.);
#4659=EDGE_CURVE('',#3786,#3787,#2096,.T.);
#4660=EDGE_CURVE('',#3787,#3788,#2097,.T.);
#4661=EDGE_CURVE('',#3788,#3789,#2098,.T.);
#4662=EDGE_CURVE('',#3789,#3790,#2099,.T.);
#4663=EDGE_CURVE('',#3790,#3791,#2100,.T.);
#4664=EDGE_CURVE('',#3791,#3782,#2101,.T.);
#4665=EDGE_CURVE('',#3792,#3793,#2102,.T.);
#4666=EDGE_CURVE('',#3793,#3794,#2103,.T.);
#4667=EDGE_CURVE('',#3794,#3795,#2104,.T.);
#4668=EDGE_CURVE('',#3795,#3796,#2105,.T.);
#4669=EDGE_CURVE('',#3796,#3797,#2106,.T.);
#4670=EDGE_CURVE('',#3797,#3798,#2107,.T.);
#4671=EDGE_CURVE('',#3798,#3799,#2108,.T.);
#4672=EDGE_CURVE('',#3799,#3800,#2109,.T.);
#4673=EDGE_CURVE('',#3800,#3801,#2110,.T.);
#4674=EDGE_CURVE('',#3801,#3792,#2111,.T.);
#4675=EDGE_CURVE('',#3802,#3803,#208,.T.);
#4676=EDGE_CURVE('',#3803,#3804,#209,.T.);
#4677=EDGE_CURVE('',#3804,#3805,#210,.T.);
#4678=EDGE_CURVE('',#3805,#3806,#211,.T.);
#4679=EDGE_CURVE('',#3806,#3807,#212,.T.);
#4680=EDGE_CURVE('',#3807,#3808,#213,.T.);
#4681=EDGE_CURVE('',#3808,#3809,#214,.T.);
#4682=EDGE_CURVE('',#3809,#3810,#215,.T.);
#4683=EDGE_CURVE('',#3810,#3811,#216,.T.);
#4684=EDGE_CURVE('',#3811,#3812,#217,.T.);
#4685=EDGE_CURVE('',#3812,#3802,#218,.T.);
#4686=EDGE_CURVE('',#3813,#3814,#2112,.T.);
#4687=EDGE_CURVE('',#3814,#3815,#2113,.T.);
#4688=EDGE_CURVE('',#3815,#3816,#2114,.T.);
#4689=EDGE_CURVE('',#3816,#3817,#2115,.T.);
#4690=EDGE_CURVE('',#3817,#3818,#2116,.T.);
#4691=EDGE_CURVE('',#3818,#3819,#2117,.T.);
#4692=EDGE_CURVE('',#3819,#3820,#2118,.T.);
#4693=EDGE_CURVE('',#3820,#3821,#2119,.T.);
#4694=EDGE_CURVE('',#3821,#3822,#2120,.T.);
#4695=EDGE_CURVE('',#3822,#3813,#2121,.T.);
#4696=EDGE_CURVE('',#3823,#3824,#219,.T.);
#4697=EDGE_CURVE('',#3824,#3825,#220,.T.);
#4698=EDGE_CURVE('',#3825,#3826,#221,.T.);
#4699=EDGE_CURVE('',#3826,#3827,#222,.T.);
#4700=EDGE_CURVE('',#3827,#3828,#223,.T.);
#4701=EDGE_CURVE('',#3828,#3829,#224,.T.);
#4702=EDGE_CURVE('',#3829,#3830,#225,.T.);
#4703=EDGE_CURVE('',#3830,#3831,#226,.T.);
#4704=EDGE_CURVE('',#3831,#3832,#227,.T.);
#4705=EDGE_CURVE('',#3832,#3833,#228,.T.);
#4706=EDGE_CURVE('',#3833,#3823,#229,.T.);
#4707=EDGE_CURVE('',#3834,#3834,#674,.T.);
#4708=EDGE_CURVE('',#3835,#3836,#230,.T.);
#4709=EDGE_CURVE('',#3836,#3837,#231,.T.);
#4710=EDGE_CURVE('',#3837,#3838,#232,.T.);
#4711=EDGE_CURVE('',#3838,#3839,#233,.T.);
#4712=EDGE_CURVE('',#3839,#3840,#234,.T.);
#4713=EDGE_CURVE('',#3840,#3841,#235,.T.);
#4714=EDGE_CURVE('',#3841,#3842,#236,.T.);
#4715=EDGE_CURVE('',#3842,#3843,#237,.T.);
#4716=EDGE_CURVE('',#3843,#3844,#238,.T.);
#4717=EDGE_CURVE('',#3844,#3845,#239,.T.);
#4718=EDGE_CURVE('',#3845,#3835,#240,.T.);
#4719=EDGE_CURVE('',#3846,#3847,#2122,.T.);
#4720=EDGE_CURVE('',#3847,#3848,#2123,.T.);
#4721=EDGE_CURVE('',#3848,#3849,#2124,.T.);
#4722=EDGE_CURVE('',#3849,#3850,#2125,.T.);
#4723=EDGE_CURVE('',#3850,#3851,#2126,.T.);
#4724=EDGE_CURVE('',#3851,#3852,#2127,.T.);
#4725=EDGE_CURVE('',#3852,#3853,#2128,.T.);
#4726=EDGE_CURVE('',#3853,#3854,#2129,.T.);
#4727=EDGE_CURVE('',#3854,#3855,#2130,.T.);
#4728=EDGE_CURVE('',#3855,#3846,#2131,.T.);
#4729=EDGE_CURVE('',#3755,#3856,#2132,.T.);
#4730=EDGE_CURVE('',#3856,#3856,#675,.T.);
#4731=EDGE_CURVE('',#3857,#3857,#676,.T.);
#4732=EDGE_CURVE('',#3857,#3858,#2133,.T.);
#4733=EDGE_CURVE('',#3858,#3859,#115,.T.);
#4734=EDGE_CURVE('',#3859,#3753,#241,.T.);
#4735=EDGE_CURVE('',#3762,#3858,#116,.T.);
#4736=EDGE_CURVE('',#3857,#3860,#2134,.T.);
#4737=EDGE_CURVE('',#3860,#3860,#677,.T.);
#4738=EDGE_CURVE('',#3721,#3775,#2135,.T.);
#4739=EDGE_CURVE('',#3774,#3861,#2136,.T.);
#4740=EDGE_CURVE('',#3861,#3862,#2137,.T.);
#4741=EDGE_CURVE('',#3862,#3722,#2138,.T.);
#4742=EDGE_CURVE('',#3862,#3863,#2139,.T.);
#4743=EDGE_CURVE('',#3863,#3723,#2140,.T.);
#4744=EDGE_CURVE('',#3861,#3864,#2141,.T.);
#4745=EDGE_CURVE('',#3864,#3863,#2142,.T.);
#4746=EDGE_CURVE('',#3859,#3714,#2143,.T.);
#4747=EDGE_CURVE('',#3760,#3865,#2144,.T.);
#4748=EDGE_CURVE('',#3865,#3714,#2145,.T.);
#4749=EDGE_CURVE('',#3761,#3865,#678,.T.);
#4750=EDGE_CURVE('',#3701,#3865,#2146,.T.);
#4751=EDGE_CURVE('',#3761,#3698,#2147,.T.);
#4752=EDGE_CURVE('',#3741,#3699,#2148,.T.);
#4753=EDGE_CURVE('',#3744,#3866,#2149,.T.);
#4754=EDGE_CURVE('',#3866,#3719,#2150,.T.);
#4755=EDGE_CURVE('',#3743,#3867,#2151,.T.);
#4756=EDGE_CURVE('',#3867,#3866,#2152,.T.);
#4757=EDGE_CURVE('',#3868,#3734,#242,.T.);
#4758=EDGE_CURVE('',#3869,#3868,#243,.T.);
#4759=EDGE_CURVE('',#3870,#3869,#244,.T.);
#4760=EDGE_CURVE('',#3871,#3870,#245,.T.);
#4761=EDGE_CURVE('',#3872,#3871,#246,.T.);
#4762=EDGE_CURVE('',#3731,#3872,#247,.T.);
#4763=EDGE_CURVE('',#3781,#3873,#2153,.T.);
#4764=EDGE_CURVE('',#3873,#3867,#2154,.T.);
#4765=EDGE_CURVE('',#3780,#3874,#2155,.T.);
#4766=EDGE_CURVE('',#3874,#3873,#2156,.T.);
#4767=EDGE_CURVE('',#3779,#3875,#2157,.T.);
#4768=EDGE_CURVE('',#3875,#3874,#2158,.T.);
#4769=EDGE_CURVE('',#3778,#3876,#2159,.T.);
#4770=EDGE_CURVE('',#3876,#3875,#2160,.T.);
#4771=EDGE_CURVE('',#3777,#3877,#2161,.T.);
#4772=EDGE_CURVE('',#3877,#3876,#2162,.T.);
#4773=EDGE_CURVE('',#3776,#3878,#2163,.T.);
#4774=EDGE_CURVE('',#3878,#3877,#2164,.T.);
#4775=EDGE_CURVE('',#3720,#3878,#2165,.T.);
#4776=EDGE_CURVE('',#3773,#3879,#2166,.T.);
#4777=EDGE_CURVE('',#3879,#3864,#2167,.T.);
#4778=EDGE_CURVE('',#3772,#3880,#2168,.T.);
#4779=EDGE_CURVE('',#3880,#3879,#2169,.T.);
#4780=EDGE_CURVE('',#3771,#3881,#2170,.T.);
#4781=EDGE_CURVE('',#3881,#3880,#2171,.T.);
#4782=EDGE_CURVE('',#3770,#3882,#2172,.T.);
#4783=EDGE_CURVE('',#3882,#3881,#2173,.T.);
#4784=EDGE_CURVE('',#3769,#3883,#2174,.T.);
#4785=EDGE_CURVE('',#3883,#3882,#2175,.T.);
#4786=EDGE_CURVE('',#3768,#3884,#2176,.T.);
#4787=EDGE_CURVE('',#3884,#3883,#2177,.T.);
#4788=EDGE_CURVE('',#3724,#3884,#2178,.T.);
#4789=EDGE_CURVE('',#3767,#3868,#2179,.T.);
#4790=EDGE_CURVE('',#3766,#3869,#2180,.T.);
#4791=EDGE_CURVE('',#3765,#3870,#2181,.T.);
#4792=EDGE_CURVE('',#3764,#3871,#2182,.T.);
#4793=EDGE_CURVE('',#3763,#3872,#2183,.T.);
#4794=EDGE_CURVE('',#3782,#3885,#2184,.T.);
#4795=EDGE_CURVE('',#3885,#3886,#2185,.T.);
#4796=EDGE_CURVE('',#3783,#3886,#2186,.T.);
#4797=EDGE_CURVE('',#3791,#3887,#2187,.T.);
#4798=EDGE_CURVE('',#3887,#3885,#2188,.T.);
#4799=EDGE_CURVE('',#3790,#3888,#2189,.T.);
#4800=EDGE_CURVE('',#3888,#3887,#2190,.T.);
#4801=EDGE_CURVE('',#3789,#3889,#2191,.T.);
#4802=EDGE_CURVE('',#3889,#3888,#2192,.T.);
#4803=EDGE_CURVE('',#3788,#3890,#2193,.T.);
#4804=EDGE_CURVE('',#3890,#3889,#2194,.T.);
#4805=EDGE_CURVE('',#3787,#3891,#2195,.T.);
#4806=EDGE_CURVE('',#3891,#3890,#2196,.T.);
#4807=EDGE_CURVE('',#3786,#3892,#2197,.T.);
#4808=EDGE_CURVE('',#3892,#3891,#2198,.T.);
#4809=EDGE_CURVE('',#3785,#3893,#2199,.T.);
#4810=EDGE_CURVE('',#3893,#3892,#2200,.T.);
#4811=EDGE_CURVE('',#3784,#3894,#2201,.T.);
#4812=EDGE_CURVE('',#3894,#3893,#2202,.T.);
#4813=EDGE_CURVE('',#3886,#3894,#2203,.T.);
#4814=EDGE_CURVE('',#3792,#3895,#2204,.T.);
#4815=EDGE_CURVE('',#3895,#3896,#2205,.T.);
#4816=EDGE_CURVE('',#3793,#3896,#2206,.T.);
#4817=EDGE_CURVE('',#3801,#3897,#2207,.T.);
#4818=EDGE_CURVE('',#3897,#3895,#2208,.T.);
#4819=EDGE_CURVE('',#3800,#3898,#2209,.T.);
#4820=EDGE_CURVE('',#3898,#3897,#2210,.T.);
#4821=EDGE_CURVE('',#3799,#3899,#2211,.T.);
#4822=EDGE_CURVE('',#3899,#3898,#2212,.T.);
#4823=EDGE_CURVE('',#3798,#3900,#2213,.T.);
#4824=EDGE_CURVE('',#3900,#3899,#2214,.T.);
#4825=EDGE_CURVE('',#3797,#3901,#2215,.T.);
#4826=EDGE_CURVE('',#3901,#3900,#2216,.T.);
#4827=EDGE_CURVE('',#3796,#3902,#2217,.T.);
#4828=EDGE_CURVE('',#3902,#3901,#2218,.T.);
#4829=EDGE_CURVE('',#3795,#3903,#2219,.T.);
#4830=EDGE_CURVE('',#3903,#3902,#2220,.T.);
#4831=EDGE_CURVE('',#3794,#3904,#2221,.T.);
#4832=EDGE_CURVE('',#3904,#3903,#2222,.T.);
#4833=EDGE_CURVE('',#3896,#3904,#2223,.T.);
#4834=EDGE_CURVE('',#3802,#3905,#2224,.T.);
#4835=EDGE_CURVE('',#3905,#3906,#248,.T.);
#4836=EDGE_CURVE('',#3803,#3906,#2225,.T.);
#4837=EDGE_CURVE('',#3812,#3907,#2226,.T.);
#4838=EDGE_CURVE('',#3907,#3905,#249,.T.);
#4839=EDGE_CURVE('',#3811,#3908,#2227,.T.);
#4840=EDGE_CURVE('',#3908,#3907,#250,.T.);
#4841=EDGE_CURVE('',#3810,#3909,#2228,.T.);
#4842=EDGE_CURVE('',#3909,#3908,#251,.T.);
#4843=EDGE_CURVE('',#3809,#3910,#2229,.T.);
#4844=EDGE_CURVE('',#3910,#3909,#252,.T.);
#4845=EDGE_CURVE('',#3808,#3911,#2230,.T.);
#4846=EDGE_CURVE('',#3911,#3910,#253,.T.);
#4847=EDGE_CURVE('',#3807,#3912,#2231,.T.);
#4848=EDGE_CURVE('',#3912,#3911,#254,.T.);
#4849=EDGE_CURVE('',#3806,#3913,#2232,.T.);
#4850=EDGE_CURVE('',#3913,#3912,#255,.T.);
#4851=EDGE_CURVE('',#3805,#3914,#2233,.T.);
#4852=EDGE_CURVE('',#3914,#3913,#256,.T.);
#4853=EDGE_CURVE('',#3804,#3915,#2234,.T.);
#4854=EDGE_CURVE('',#3915,#3914,#257,.T.);
#4855=EDGE_CURVE('',#3906,#3915,#258,.T.);
#4856=EDGE_CURVE('',#3846,#3916,#2235,.T.);
#4857=EDGE_CURVE('',#3916,#3917,#2236,.T.);
#4858=EDGE_CURVE('',#3847,#3917,#2237,.T.);
#4859=EDGE_CURVE('',#3855,#3918,#2238,.T.);
#4860=EDGE_CURVE('',#3918,#3916,#2239,.T.);
#4861=EDGE_CURVE('',#3854,#3919,#2240,.T.);
#4862=EDGE_CURVE('',#3919,#3918,#2241,.T.);
#4863=EDGE_CURVE('',#3853,#3920,#2242,.T.);
#4864=EDGE_CURVE('',#3920,#3919,#2243,.T.);
#4865=EDGE_CURVE('',#3852,#3921,#2244,.T.);
#4866=EDGE_CURVE('',#3921,#3920,#2245,.T.);
#4867=EDGE_CURVE('',#3851,#3922,#2246,.T.);
#4868=EDGE_CURVE('',#3922,#3921,#2247,.T.);
#4869=EDGE_CURVE('',#3850,#3923,#2248,.T.);
#4870=EDGE_CURVE('',#3923,#3922,#2249,.T.);
#4871=EDGE_CURVE('',#3849,#3924,#2250,.T.);
#4872=EDGE_CURVE('',#3924,#3923,#2251,.T.);
#4873=EDGE_CURVE('',#3848,#3925,#2252,.T.);
#4874=EDGE_CURVE('',#3925,#3924,#2253,.T.);
#4875=EDGE_CURVE('',#3917,#3925,#2254,.T.);
#4876=EDGE_CURVE('',#3835,#3926,#2255,.T.);
#4877=EDGE_CURVE('',#3926,#3927,#259,.T.);
#4878=EDGE_CURVE('',#3836,#3927,#2256,.T.);
#4879=EDGE_CURVE('',#3845,#3928,#2257,.T.);
#4880=EDGE_CURVE('',#3928,#3926,#260,.T.);
#4881=EDGE_CURVE('',#3844,#3929,#2258,.T.);
#4882=EDGE_CURVE('',#3929,#3928,#261,.T.);
#4883=EDGE_CURVE('',#3843,#3930,#2259,.T.);
#4884=EDGE_CURVE('',#3930,#3929,#262,.T.);
#4885=EDGE_CURVE('',#3842,#3931,#2260,.T.);
#4886=EDGE_CURVE('',#3931,#3930,#263,.T.);
#4887=EDGE_CURVE('',#3841,#3932,#2261,.T.);
#4888=EDGE_CURVE('',#3932,#3931,#264,.T.);
#4889=EDGE_CURVE('',#3840,#3933,#2262,.T.);
#4890=EDGE_CURVE('',#3933,#3932,#265,.T.);
#4891=EDGE_CURVE('',#3839,#3934,#2263,.T.);
#4892=EDGE_CURVE('',#3934,#3933,#266,.T.);
#4893=EDGE_CURVE('',#3838,#3935,#2264,.T.);
#4894=EDGE_CURVE('',#3935,#3934,#267,.T.);
#4895=EDGE_CURVE('',#3837,#3936,#2265,.T.);
#4896=EDGE_CURVE('',#3936,#3935,#268,.T.);
#4897=EDGE_CURVE('',#3927,#3936,#269,.T.);
#4898=EDGE_CURVE('',#3813,#3937,#2266,.T.);
#4899=EDGE_CURVE('',#3937,#3938,#2267,.T.);
#4900=EDGE_CURVE('',#3814,#3938,#2268,.T.);
#4901=EDGE_CURVE('',#3822,#3939,#2269,.T.);
#4902=EDGE_CURVE('',#3939,#3937,#2270,.T.);
#4903=EDGE_CURVE('',#3821,#3940,#2271,.T.);
#4904=EDGE_CURVE('',#3940,#3939,#2272,.T.);
#4905=EDGE_CURVE('',#3820,#3941,#2273,.T.);
#4906=EDGE_CURVE('',#3941,#3940,#2274,.T.);
#4907=EDGE_CURVE('',#3819,#3942,#2275,.T.);
#4908=EDGE_CURVE('',#3942,#3941,#2276,.T.);
#4909=EDGE_CURVE('',#3818,#3943,#2277,.T.);
#4910=EDGE_CURVE('',#3943,#3942,#2278,.T.);
#4911=EDGE_CURVE('',#3817,#3944,#2279,.T.);
#4912=EDGE_CURVE('',#3944,#3943,#2280,.T.);
#4913=EDGE_CURVE('',#3816,#3945,#2281,.T.);
#4914=EDGE_CURVE('',#3945,#3944,#2282,.T.);
#4915=EDGE_CURVE('',#3815,#3946,#2283,.T.);
#4916=EDGE_CURVE('',#3946,#3945,#2284,.T.);
#4917=EDGE_CURVE('',#3938,#3946,#2285,.T.);
#4918=EDGE_CURVE('',#3823,#3947,#2286,.T.);
#4919=EDGE_CURVE('',#3947,#3948,#270,.T.);
#4920=EDGE_CURVE('',#3824,#3948,#2287,.T.);
#4921=EDGE_CURVE('',#3833,#3949,#2288,.T.);
#4922=EDGE_CURVE('',#3949,#3947,#271,.T.);
#4923=EDGE_CURVE('',#3832,#3950,#2289,.T.);
#4924=EDGE_CURVE('',#3950,#3949,#272,.T.);
#4925=EDGE_CURVE('',#3831,#3951,#2290,.T.);
#4926=EDGE_CURVE('',#3951,#3950,#273,.T.);
#4927=EDGE_CURVE('',#3830,#3952,#2291,.T.);
#4928=EDGE_CURVE('',#3952,#3951,#274,.T.);
#4929=EDGE_CURVE('',#3829,#3953,#2292,.T.);
#4930=EDGE_CURVE('',#3953,#3952,#275,.T.);
#4931=EDGE_CURVE('',#3828,#3954,#2293,.T.);
#4932=EDGE_CURVE('',#3954,#3953,#276,.T.);
#4933=EDGE_CURVE('',#3827,#3955,#2294,.T.);
#4934=EDGE_CURVE('',#3955,#3954,#277,.T.);
#4935=EDGE_CURVE('',#3826,#3956,#2295,.T.);
#4936=EDGE_CURVE('',#3956,#3955,#278,.T.);
#4937=EDGE_CURVE('',#3825,#3957,#2296,.T.);
#4938=EDGE_CURVE('',#3957,#3956,#279,.T.);
#4939=EDGE_CURVE('',#3948,#3957,#280,.T.);
#4940=EDGE_CURVE('',#3860,#3696,#2297,.T.);
#4941=EDGE_CURVE('',#3745,#3695,#2298,.T.);
#4942=EDGE_CURVE('',#3856,#3694,#2299,.T.);
#4943=EDGE_CURVE('',#3754,#3693,#2300,.T.);
#4944=EDGE_CURVE('',#3834,#3697,#2301,.T.);
#4945=EDGE_CURVE('',#3686,#3705,#2302,.T.);
#4946=EDGE_CURVE('',#3709,#3684,#2303,.T.);
#4947=EDGE_CURVE('',#3958,#3959,#2304,.T.);
#4948=EDGE_CURVE('',#3959,#3960,#2305,.T.);
#4949=EDGE_CURVE('',#3960,#3961,#2306,.T.);
#4950=EDGE_CURVE('',#3961,#3958,#2307,.T.);
#4951=EDGE_CURVE('',#3962,#3963,#2308,.T.);
#4952=EDGE_CURVE('',#3963,#3959,#679,.T.);
#4953=EDGE_CURVE('',#3958,#3962,#680,.T.);
#4954=EDGE_CURVE('',#3964,#3965,#2309,.T.);
#4955=EDGE_CURVE('',#3965,#3963,#2310,.T.);
#4956=EDGE_CURVE('',#3962,#3964,#2311,.T.);
#4957=EDGE_CURVE('',#3966,#3967,#2312,.T.);
#4958=EDGE_CURVE('',#3967,#3965,#681,.T.);
#4959=EDGE_CURVE('',#3964,#3966,#682,.T.);
#4960=EDGE_CURVE('',#3968,#3969,#2313,.T.);
#4961=EDGE_CURVE('',#3969,#3967,#2314,.T.);
#4962=EDGE_CURVE('',#3966,#3968,#2315,.T.);
#4963=EDGE_CURVE('',#3970,#3971,#2316,.T.);
#4964=EDGE_CURVE('',#3971,#3969,#683,.T.);
#4965=EDGE_CURVE('',#3968,#3970,#684,.T.);
#4966=EDGE_CURVE('',#3972,#3973,#2317,.T.);
#4967=EDGE_CURVE('',#3973,#3971,#2318,.T.);
#4968=EDGE_CURVE('',#3970,#3972,#2319,.T.);
#4969=EDGE_CURVE('',#3960,#3973,#685,.T.);
#4970=EDGE_CURVE('',#3972,#3961,#686,.T.);
#4971=EDGE_CURVE('',#3971,#3974,#2320,.T.);
#4972=EDGE_CURVE('',#3975,#3974,#687,.T.);
#4973=EDGE_CURVE('',#3975,#3969,#2321,.T.);
#4974=EDGE_CURVE('',#3976,#3973,#2322,.T.);
#4975=EDGE_CURVE('',#3974,#3976,#2323,.T.);
#4976=EDGE_CURVE('',#3960,#3977,#2324,.T.);
#4977=EDGE_CURVE('',#3976,#3977,#688,.T.);
#4978=EDGE_CURVE('',#3978,#3959,#2325,.T.);
#4979=EDGE_CURVE('',#3977,#3978,#2326,.T.);
#4980=EDGE_CURVE('',#3979,#3979,#689,.T.);
#4981=EDGE_CURVE('',#3980,#3980,#690,.T.);
#4982=EDGE_CURVE('',#3981,#3981,#691,.T.);
#4983=EDGE_CURVE('',#3982,#3982,#692,.T.);
#4984=EDGE_CURVE('',#3983,#3983,#693,.T.);
#4985=EDGE_CURVE('',#3984,#3984,#694,.T.);
#4986=EDGE_CURVE('',#3984,#3985,#2327,.T.);
#4987=EDGE_CURVE('',#3985,#3985,#695,.T.);
#4988=EDGE_CURVE('',#3986,#3987,#2328,.T.);
#4989=EDGE_CURVE('',#3988,#3986,#696,.T.);
#4990=EDGE_CURVE('',#3989,#3988,#2329,.T.);
#4991=EDGE_CURVE('',#3990,#3989,#697,.T.);
#4992=EDGE_CURVE('',#3991,#3990,#2330,.T.);
#4993=EDGE_CURVE('',#3992,#3991,#698,.T.);
#4994=EDGE_CURVE('',#3993,#3992,#2331,.T.);
#4995=EDGE_CURVE('',#3987,#3993,#699,.T.);
#4996=EDGE_CURVE('',#3994,#3994,#700,.T.);
#4997=EDGE_CURVE('',#3995,#3995,#701,.T.);
#4998=EDGE_CURVE('',#3996,#3996,#702,.T.);
#4999=EDGE_CURVE('',#3997,#3997,#703,.T.);
#5000=EDGE_CURVE('',#3984,#3998,#2332,.T.);
#5001=EDGE_CURVE('',#3998,#3998,#704,.T.);
#5002=EDGE_CURVE('',#3999,#3986,#2333,.T.);
#5003=EDGE_CURVE('',#3987,#4000,#2334,.T.);
#5004=EDGE_CURVE('',#4000,#3999,#2335,.T.);
#5005=EDGE_CURVE('',#3999,#4001,#705,.T.);
#5006=EDGE_CURVE('',#4001,#3988,#2336,.T.);
#5007=EDGE_CURVE('',#3975,#3989,#2337,.T.);
#5008=EDGE_CURVE('',#4001,#3975,#2338,.T.);
#5009=EDGE_CURVE('',#3974,#3990,#2339,.T.);
#5010=EDGE_CURVE('',#3976,#3991,#2340,.T.);
#5011=EDGE_CURVE('',#3977,#3992,#2341,.T.);
#5012=EDGE_CURVE('',#3978,#3993,#2342,.T.);
#5013=EDGE_CURVE('',#3978,#4000,#706,.T.);
#5014=EDGE_CURVE('',#3967,#4001,#2343,.T.);
#5015=EDGE_CURVE('',#3999,#3965,#2344,.T.);
#5016=EDGE_CURVE('',#3963,#4000,#2345,.T.);
#5017=EDGE_CURVE('',#4002,#4002,#707,.T.);
#5018=EDGE_CURVE('',#4002,#3997,#2346,.T.);
#5019=EDGE_CURVE('',#4002,#4003,#2347,.T.);
#5020=EDGE_CURVE('',#4003,#4003,#708,.T.);
#5021=EDGE_CURVE('',#4004,#4004,#709,.T.);
#5022=EDGE_CURVE('',#4004,#3994,#2348,.T.);
#5023=EDGE_CURVE('',#4004,#4005,#2349,.T.);
#5024=EDGE_CURVE('',#4005,#4005,#710,.T.);
#5025=EDGE_CURVE('',#4006,#4006,#711,.T.);
#5026=EDGE_CURVE('',#4006,#3996,#2350,.T.);
#5027=EDGE_CURVE('',#4006,#4007,#2351,.T.);
#5028=EDGE_CURVE('',#4007,#4007,#712,.T.);
#5029=EDGE_CURVE('',#4007,#3982,#2352,.T.);
#5030=EDGE_CURVE('',#4005,#3981,#2353,.T.);
#5031=EDGE_CURVE('',#3998,#3980,#2354,.T.);
#5032=EDGE_CURVE('',#4003,#3979,#2355,.T.);
#5033=EDGE_CURVE('',#3995,#3983,#2356,.T.);
#5034=EDGE_CURVE('',#4008,#4008,#713,.T.);
#5035=EDGE_CURVE('',#4008,#4009,#2357,.T.);
#5036=EDGE_CURVE('',#4009,#4009,#714,.T.);
#5037=EDGE_CURVE('',#4010,#4011,#2358,.T.);
#5038=EDGE_CURVE('',#4012,#4010,#2359,.T.);
#5039=EDGE_CURVE('',#4013,#4012,#2360,.T.);
#5040=EDGE_CURVE('',#4014,#4013,#2361,.T.);
#5041=EDGE_CURVE('',#4015,#4014,#2362,.T.);
#5042=EDGE_CURVE('',#4016,#4015,#2363,.T.);
#5043=EDGE_CURVE('',#4017,#4016,#2364,.T.);
#5044=EDGE_CURVE('',#4018,#4017,#2365,.T.);
#5045=EDGE_CURVE('',#4019,#4018,#2366,.T.);
#5046=EDGE_CURVE('',#4020,#4019,#2367,.T.);
#5047=EDGE_CURVE('',#4021,#4020,#2368,.T.);
#5048=EDGE_CURVE('',#4022,#4021,#2369,.T.);
#5049=EDGE_CURVE('',#4023,#4022,#2370,.T.);
#5050=EDGE_CURVE('',#4024,#4023,#2371,.T.);
#5051=EDGE_CURVE('',#4025,#4024,#2372,.T.);
#5052=EDGE_CURVE('',#4026,#4025,#2373,.T.);
#5053=EDGE_CURVE('',#4027,#4026,#2374,.T.);
#5054=EDGE_CURVE('',#4028,#4027,#2375,.T.);
#5055=EDGE_CURVE('',#4029,#4028,#2376,.T.);
#5056=EDGE_CURVE('',#4030,#4029,#2377,.T.);
#5057=EDGE_CURVE('',#4031,#4030,#2378,.T.);
#5058=EDGE_CURVE('',#4032,#4031,#2379,.T.);
#5059=EDGE_CURVE('',#4032,#4033,#715,.T.);
#5060=EDGE_CURVE('',#4011,#4033,#2380,.T.);
#5061=EDGE_CURVE('',#4034,#4034,#716,.T.);
#5062=EDGE_CURVE('',#4009,#4035,#2381,.T.);
#5063=EDGE_CURVE('',#4035,#4035,#717,.T.);
#5064=EDGE_CURVE('',#4034,#4036,#2382,.T.);
#5065=EDGE_CURVE('',#4036,#4036,#718,.T.);
#5066=EDGE_CURVE('',#4036,#4037,#2383,.T.);
#5067=EDGE_CURVE('',#4037,#4037,#719,.T.);
#5068=EDGE_CURVE('',#4038,#4039,#2384,.T.);
#5069=EDGE_CURVE('',#4039,#4040,#2385,.T.);
#5070=EDGE_CURVE('',#4040,#4041,#2386,.T.);
#5071=EDGE_CURVE('',#4041,#4042,#2387,.T.);
#5072=EDGE_CURVE('',#4042,#4043,#2388,.T.);
#5073=EDGE_CURVE('',#4043,#4038,#2389,.T.);
#5074=EDGE_CURVE('',#4044,#4039,#2390,.T.);
#5075=EDGE_CURVE('',#4045,#4044,#2391,.T.);
#5076=EDGE_CURVE('',#4040,#4045,#2392,.T.);
#5077=EDGE_CURVE('',#4046,#4038,#2393,.T.);
#5078=EDGE_CURVE('',#4046,#4047,#2394,.T.);
#5079=EDGE_CURVE('',#4047,#4048,#2395,.T.);
#5080=EDGE_CURVE('',#4044,#4048,#2396,.T.);
#5081=EDGE_CURVE('',#4043,#4049,#2397,.T.);
#5082=EDGE_CURVE('',#4049,#4050,#2398,.T.);
#5083=EDGE_CURVE('',#4050,#4046,#2399,.T.);
#5084=EDGE_CURVE('',#4051,#4045,#2400,.T.);
#5085=EDGE_CURVE('',#4048,#4052,#2401,.T.);
#5086=EDGE_CURVE('',#4052,#4053,#2402,.T.);
#5087=EDGE_CURVE('',#4053,#4051,#2403,.T.);
#5088=EDGE_CURVE('',#4012,#4051,#2404,.T.);
#5089=EDGE_CURVE('',#4041,#4010,#2405,.T.);
#5090=EDGE_CURVE('',#4053,#4054,#2406,.T.);
#5091=EDGE_CURVE('',#4013,#4054,#2407,.T.);
#5092=EDGE_CURVE('',#4055,#4055,#720,.T.);
#5093=EDGE_CURVE('',#4055,#4056,#2408,.T.);
#5094=EDGE_CURVE('',#4056,#4056,#721,.T.);
#5095=EDGE_CURVE('',#4057,#4050,#2409,.T.);
#5096=EDGE_CURVE('',#4057,#4058,#722,.T.);
#5097=EDGE_CURVE('',#4059,#4058,#2410,.T.);
#5098=EDGE_CURVE('',#4060,#4059,#2411,.T.);
#5099=EDGE_CURVE('',#4061,#4060,#2412,.T.);
#5100=EDGE_CURVE('',#4062,#4061,#2413,.T.);
#5101=EDGE_CURVE('',#4063,#4062,#2414,.T.);
#5102=EDGE_CURVE('',#4064,#4063,#2415,.T.);
#5103=EDGE_CURVE('',#4065,#4064,#2416,.T.);
#5104=EDGE_CURVE('',#4066,#4065,#2417,.T.);
#5105=EDGE_CURVE('',#4067,#4066,#2418,.T.);
#5106=EDGE_CURVE('',#4068,#4067,#2419,.T.);
#5107=EDGE_CURVE('',#4069,#4068,#2420,.T.);
#5108=EDGE_CURVE('',#4070,#4069,#2421,.T.);
#5109=EDGE_CURVE('',#4071,#4070,#2422,.T.);
#5110=EDGE_CURVE('',#4072,#4071,#2423,.T.);
#5111=EDGE_CURVE('',#4073,#4072,#2424,.T.);
#5112=EDGE_CURVE('',#4074,#4073,#2425,.T.);
#5113=EDGE_CURVE('',#4075,#4074,#2426,.T.);
#5114=EDGE_CURVE('',#4076,#4075,#2427,.T.);
#5115=EDGE_CURVE('',#4077,#4076,#2428,.T.);
#5116=EDGE_CURVE('',#4047,#4077,#2429,.T.);
#5117=EDGE_CURVE('',#4078,#4078,#723,.T.);
#5118=EDGE_CURVE('',#4056,#4079,#2430,.T.);
#5119=EDGE_CURVE('',#4079,#4079,#724,.T.);
#5120=EDGE_CURVE('',#4078,#4080,#2431,.T.);
#5121=EDGE_CURVE('',#4080,#4080,#725,.T.);
#5122=EDGE_CURVE('',#4080,#4081,#2432,.T.);
#5123=EDGE_CURVE('',#4081,#4081,#726,.T.);
#5124=EDGE_CURVE('',#4082,#4083,#2433,.T.);
#5125=EDGE_CURVE('',#4011,#4082,#2434,.T.);
#5126=EDGE_CURVE('',#4083,#4011,#2435,.T.);
#5127=EDGE_CURVE('',#4082,#4042,#2436,.T.);
#5128=EDGE_CURVE('',#4033,#4084,#830,.T.);
#5129=EDGE_CURVE('',#4084,#4083,#2437,.T.);
#5130=EDGE_CURVE('',#4085,#4049,#2438,.T.);
#5131=EDGE_CURVE('',#4050,#4085,#2439,.T.);
#5132=EDGE_CURVE('',#4049,#4082,#2440,.T.);
#5133=EDGE_CURVE('',#4083,#4085,#2441,.T.);
#5134=EDGE_CURVE('',#4086,#4057,#831,.T.);
#5135=EDGE_CURVE('',#4085,#4086,#2442,.T.);
#5136=EDGE_CURVE('',#4031,#4087,#2443,.T.);
#5137=EDGE_CURVE('',#4088,#4031,#2444,.T.);
#5138=EDGE_CURVE('',#4087,#4088,#2445,.T.);
#5139=EDGE_CURVE('',#4089,#4090,#2446,.T.);
#5140=EDGE_CURVE('',#4090,#4088,#2447,.T.);
#5141=EDGE_CURVE('',#4030,#4089,#2448,.T.);
#5142=EDGE_CURVE('',#4091,#4059,#2449,.T.);
#5143=EDGE_CURVE('',#4092,#4091,#2450,.T.);
#5144=EDGE_CURVE('',#4059,#4092,#2451,.T.);
#5145=EDGE_CURVE('',#4091,#4087,#2452,.T.);
#5146=EDGE_CURVE('',#4088,#4092,#2453,.T.);
#5147=EDGE_CURVE('',#4093,#4060,#2454,.T.);
#5148=EDGE_CURVE('',#4092,#4094,#2455,.T.);
#5149=EDGE_CURVE('',#4094,#4093,#2456,.T.);
#5150=EDGE_CURVE('',#4058,#4095,#832,.T.);
#5151=EDGE_CURVE('',#4095,#4091,#2457,.T.);
#5152=EDGE_CURVE('',#4096,#4032,#833,.T.);
#5153=EDGE_CURVE('',#4087,#4096,#2458,.T.);
#5154=EDGE_CURVE('',#4095,#4096,#2459,.T.);
#5155=EDGE_CURVE('',#4097,#4097,#727,.T.);
#5156=EDGE_CURVE('',#4098,#4098,#728,.T.);
#5157=EDGE_CURVE('',#4099,#4099,#729,.T.);
#5158=EDGE_CURVE('',#4084,#4086,#2460,.T.);
#5159=EDGE_CURVE('',#4093,#4100,#2461,.T.);
#5160=EDGE_CURVE('',#4061,#4100,#2462,.T.);
#5161=EDGE_CURVE('',#4101,#4102,#2463,.T.);
#5162=EDGE_CURVE('',#4102,#4072,#2464,.T.);
#5163=EDGE_CURVE('',#4071,#4101,#2465,.T.);
#5164=EDGE_CURVE('',#4077,#4103,#2466,.T.);
#5165=EDGE_CURVE('',#4103,#4052,#2467,.T.);
#5166=EDGE_CURVE('',#4076,#4104,#2468,.T.);
#5167=EDGE_CURVE('',#4104,#4103,#2469,.T.);
#5168=EDGE_CURVE('',#4075,#4105,#2470,.T.);
#5169=EDGE_CURVE('',#4105,#4104,#2471,.T.);
#5170=EDGE_CURVE('',#4106,#4105,#2472,.T.);
#5171=EDGE_CURVE('',#4074,#4106,#2473,.T.);
#5172=EDGE_CURVE('',#4107,#4106,#2474,.T.);
#5173=EDGE_CURVE('',#4073,#4107,#2475,.T.);
#5174=EDGE_CURVE('',#4102,#4107,#2476,.T.);
#5175=EDGE_CURVE('',#4108,#4101,#2477,.T.);
#5176=EDGE_CURVE('',#4070,#4108,#2478,.T.);
#5177=EDGE_CURVE('',#4109,#4108,#2479,.T.);
#5178=EDGE_CURVE('',#4069,#4109,#2480,.T.);
#5179=EDGE_CURVE('',#4110,#4109,#2481,.T.);
#5180=EDGE_CURVE('',#4068,#4110,#2482,.T.);
#5181=EDGE_CURVE('',#4111,#4110,#2483,.T.);
#5182=EDGE_CURVE('',#4067,#4111,#2484,.T.);
#5183=EDGE_CURVE('',#4112,#4111,#2485,.T.);
#5184=EDGE_CURVE('',#4066,#4112,#2486,.T.);
#5185=EDGE_CURVE('',#4113,#4112,#2487,.T.);
#5186=EDGE_CURVE('',#4065,#4113,#2488,.T.);
#5187=EDGE_CURVE('',#4114,#4113,#2489,.T.);
#5188=EDGE_CURVE('',#4064,#4114,#2490,.T.);
#5189=EDGE_CURVE('',#4115,#4114,#2491,.T.);
#5190=EDGE_CURVE('',#4063,#4115,#2492,.T.);
#5191=EDGE_CURVE('',#4116,#4115,#2493,.T.);
#5192=EDGE_CURVE('',#4062,#4116,#2494,.T.);
#5193=EDGE_CURVE('',#4100,#4116,#2495,.T.);
#5194=EDGE_CURVE('',#4112,#4117,#2496,.T.);
#5195=EDGE_CURVE('',#4118,#4117,#2497,.T.);
#5196=EDGE_CURVE('',#4118,#4111,#2498,.T.);
#5197=EDGE_CURVE('',#4119,#4113,#2499,.T.);
#5198=EDGE_CURVE('',#4117,#4119,#2500,.T.);
#5199=EDGE_CURVE('',#4120,#4114,#2501,.T.);
#5200=EDGE_CURVE('',#4119,#4120,#2502,.T.);
#5201=EDGE_CURVE('',#4121,#4115,#2503,.T.);
#5202=EDGE_CURVE('',#4120,#4121,#2504,.T.);
#5203=EDGE_CURVE('',#4116,#4122,#2505,.T.);
#5204=EDGE_CURVE('',#4121,#4122,#2506,.T.);
#5205=EDGE_CURVE('',#4123,#4100,#2507,.T.);
#5206=EDGE_CURVE('',#4122,#4123,#2508,.T.);
#5207=EDGE_CURVE('',#4123,#4089,#2509,.T.);
#5208=EDGE_CURVE('',#4094,#4090,#2510,.T.);
#5209=EDGE_CURVE('',#4029,#4123,#2511,.T.);
#5210=EDGE_CURVE('',#4028,#4122,#2512,.T.);
#5211=EDGE_CURVE('',#4027,#4121,#2513,.T.);
#5212=EDGE_CURVE('',#4026,#4120,#2514,.T.);
#5213=EDGE_CURVE('',#4025,#4119,#2515,.T.);
#5214=EDGE_CURVE('',#4024,#4117,#2516,.T.);
#5215=EDGE_CURVE('',#4023,#4118,#2517,.T.);
#5216=EDGE_CURVE('',#4022,#4124,#2518,.T.);
#5217=EDGE_CURVE('',#4124,#4118,#2519,.T.);
#5218=EDGE_CURVE('',#4021,#4125,#2520,.T.);
#5219=EDGE_CURVE('',#4125,#4124,#2521,.T.);
#5220=EDGE_CURVE('',#4020,#4126,#2522,.T.);
#5221=EDGE_CURVE('',#4126,#4125,#2523,.T.);
#5222=EDGE_CURVE('',#4019,#4127,#2524,.T.);
#5223=EDGE_CURVE('',#4127,#4126,#2525,.T.);
#5224=EDGE_CURVE('',#4018,#4128,#2526,.T.);
#5225=EDGE_CURVE('',#4128,#4127,#2527,.T.);
#5226=EDGE_CURVE('',#4016,#4129,#2528,.T.);
#5227=EDGE_CURVE('',#4129,#4130,#2529,.T.);
#5228=EDGE_CURVE('',#4130,#4017,#2530,.T.);
#5229=EDGE_CURVE('',#4131,#4129,#2531,.T.);
#5230=EDGE_CURVE('',#4015,#4131,#2532,.T.);
#5231=EDGE_CURVE('',#4132,#4131,#2533,.T.);
#5232=EDGE_CURVE('',#4014,#4132,#2534,.T.);
#5233=EDGE_CURVE('',#4130,#4128,#2535,.T.);
#5234=EDGE_CURVE('',#4054,#4132,#2536,.T.);
#5235=EDGE_CURVE('',#4110,#4124,#2537,.T.);
#5236=EDGE_CURVE('',#4125,#4109,#2538,.T.);
#5237=EDGE_CURVE('',#4108,#4126,#2539,.T.);
#5238=EDGE_CURVE('',#4133,#4133,#730,.T.);
#5239=EDGE_CURVE('',#4134,#4134,#731,.T.);
#5240=EDGE_CURVE('',#4135,#4135,#732,.T.);
#5241=EDGE_CURVE('',#4127,#4101,#2540,.T.);
#5242=EDGE_CURVE('',#4128,#4102,#2541,.T.);
#5243=EDGE_CURVE('',#4130,#4107,#2542,.T.);
#5244=EDGE_CURVE('',#4106,#4129,#2543,.T.);
#5245=EDGE_CURVE('',#4131,#4105,#2544,.T.);
#5246=EDGE_CURVE('',#4104,#4132,#2545,.T.);
#5247=EDGE_CURVE('',#4054,#4103,#2546,.T.);
#5248=EDGE_CURVE('',#4133,#4099,#2547,.T.);
#5249=EDGE_CURVE('',#4134,#4098,#2548,.T.);
#5250=EDGE_CURVE('',#4135,#4097,#2549,.T.);
#5251=EDGE_CURVE('',#4136,#4136,#733,.T.);
#5252=EDGE_CURVE('',#4137,#4137,#734,.T.);
#5253=EDGE_CURVE('',#4137,#4136,#2550,.T.);
#5254=EDGE_CURVE('',#4138,#4138,#735,.T.);
#5255=EDGE_CURVE('',#4138,#4137,#2551,.T.);
#5256=EDGE_CURVE('',#4139,#4139,#736,.T.);
#5257=EDGE_CURVE('',#4139,#4138,#2552,.T.);
#5258=EDGE_CURVE('',#4140,#4140,#737,.T.);
#5259=EDGE_CURVE('',#4140,#4141,#2553,.T.);
#5260=EDGE_CURVE('',#4141,#4142,#738,.T.);
#5261=EDGE_CURVE('',#4142,#4141,#739,.T.);
#5262=EDGE_CURVE('',#4142,#4143,#2554,.T.);
#5263=EDGE_CURVE('',#4143,#4143,#740,.T.);
#5264=EDGE_CURVE('',#4144,#4145,#117,.T.);
#5265=EDGE_CURVE('',#4145,#4146,#2555,.T.);
#5266=EDGE_CURVE('',#4146,#4147,#118,.T.);
#5267=EDGE_CURVE('',#4147,#4144,#2556,.T.);
#5268=EDGE_CURVE('',#4146,#4145,#741,.T.);
#5269=EDGE_CURVE('',#4148,#4144,#742,.T.);
#5270=EDGE_CURVE('',#4147,#4148,#743,.T.);
#5271=EDGE_CURVE('',#4149,#4150,#744,.T.);
#5272=EDGE_CURVE('',#4150,#4149,#2557,.T.);
#5273=EDGE_CURVE('',#4150,#4147,#2558,.T.);
#5274=EDGE_CURVE('',#4144,#4149,#2559,.T.);
#5275=EDGE_CURVE('',#4151,#4151,#745,.T.);
#5276=EDGE_CURVE('',#4151,#4148,#2560,.T.);
#5277=EDGE_CURVE('',#4152,#4152,#746,.T.);
#5278=EDGE_CURVE('',#4143,#4152,#2561,.T.);
#5279=EDGE_CURVE('',#4153,#4154,#747,.T.);
#5280=EDGE_CURVE('',#4154,#4153,#748,.T.);
#5281=EDGE_CURVE('',#4153,#4155,#2562,.T.);
#5282=EDGE_CURVE('',#4155,#4155,#749,.T.);
#5283=EDGE_CURVE('',#4156,#4156,#750,.T.);
#5284=EDGE_CURVE('',#4156,#4154,#2563,.T.);
#5285=EDGE_CURVE('',#4157,#4157,#751,.T.);
#5286=EDGE_CURVE('',#4157,#4156,#2564,.T.);
#5287=EDGE_CURVE('',#4158,#4158,#752,.T.);
#5288=EDGE_CURVE('',#4159,#4159,#753,.T.);
#5289=EDGE_CURVE('',#4159,#4158,#2565,.T.);
#5290=EDGE_CURVE('',#4160,#4160,#754,.T.);
#5291=EDGE_CURVE('',#4160,#4159,#2566,.T.);
#5292=EDGE_CURVE('',#4161,#4162,#755,.T.);
#5293=EDGE_CURVE('',#4162,#4161,#756,.T.);
#5294=EDGE_CURVE('',#4161,#4163,#2567,.T.);
#5295=EDGE_CURVE('',#4163,#4163,#757,.T.);
#5296=EDGE_CURVE('',#4164,#4164,#758,.T.);
#5297=EDGE_CURVE('',#4165,#4165,#759,.T.);
#5298=EDGE_CURVE('',#4165,#4162,#2568,.T.);
#5299=EDGE_CURVE('',#4166,#4166,#760,.T.);
#5300=EDGE_CURVE('',#4166,#4164,#2569,.T.);
#5301=EDGE_CURVE('',#4167,#4167,#761,.T.);
#5302=EDGE_CURVE('',#4168,#4168,#762,.T.);
#5303=EDGE_CURVE('',#4168,#4167,#2570,.T.);
#5304=EDGE_CURVE('',#4169,#4170,#2571,.T.);
#5305=EDGE_CURVE('',#4170,#4171,#763,.T.);
#5306=EDGE_CURVE('',#4172,#4171,#2572,.T.);
#5307=EDGE_CURVE('',#4172,#4169,#764,.T.);
#5308=EDGE_CURVE('',#4169,#4173,#2573,.T.);
#5309=EDGE_CURVE('',#4174,#4173,#834,.T.);
#5310=EDGE_CURVE('',#4174,#4170,#2574,.T.);
#5311=EDGE_CURVE('',#4175,#4172,#2575,.T.);
#5312=EDGE_CURVE('',#4176,#4175,#765,.T.);
#5313=EDGE_CURVE('',#4177,#4176,#2576,.T.);
#5314=EDGE_CURVE('',#4177,#4173,#766,.T.);
#5315=EDGE_CURVE('',#4175,#4178,#2577,.T.);
#5316=EDGE_CURVE('',#4178,#4179,#767,.T.);
#5317=EDGE_CURVE('',#4176,#4179,#2578,.T.);
#5318=EDGE_CURVE('',#4171,#4178,#2579,.T.);
#5319=EDGE_CURVE('',#4180,#4181,#2580,.T.);
#5320=EDGE_CURVE('',#4181,#4182,#768,.T.);
#5321=EDGE_CURVE('',#4183,#4182,#2581,.T.);
#5322=EDGE_CURVE('',#4183,#4180,#769,.T.);
#5323=EDGE_CURVE('',#4180,#4184,#2582,.T.);
#5324=EDGE_CURVE('',#4184,#4185,#2583,.T.);
#5325=EDGE_CURVE('',#4185,#4181,#2584,.T.);
#5326=EDGE_CURVE('',#4186,#4183,#2585,.T.);
#5327=EDGE_CURVE('',#4186,#4187,#770,.T.);
#5328=EDGE_CURVE('',#4188,#4187,#2586,.T.);
#5329=EDGE_CURVE('',#4184,#4188,#771,.T.);
#5330=EDGE_CURVE('',#4188,#4189,#2587,.T.);
#5331=EDGE_CURVE('',#4189,#4185,#772,.T.);
#5332=EDGE_CURVE('',#4190,#4187,#835,.T.);
#5333=EDGE_CURVE('',#4190,#4189,#2588,.T.);
#5334=EDGE_CURVE('',#4191,#4192,#2589,.T.);
#5335=EDGE_CURVE('',#4192,#4192,#281,.T.);
#5336=EDGE_CURVE('',#4191,#4191,#282,.T.);
#5337=EDGE_CURVE('',#4192,#4193,#2590,.T.);
#5338=EDGE_CURVE('',#4194,#4193,#283,.T.);
#5339=EDGE_CURVE('',#4193,#4194,#284,.T.);
#5340=EDGE_CURVE('',#4174,#4195,#836,.T.);
#5341=EDGE_CURVE('',#4196,#4177,#837,.F.);
#5342=EDGE_CURVE('',#4197,#4196,#838,.T.);
#5343=EDGE_CURVE('',#4198,#4197,#773,.T.);
#5344=EDGE_CURVE('',#4198,#4199,#2591,.T.);
#5345=EDGE_CURVE('',#4199,#4199,#774,.T.);
#5346=EDGE_CURVE('',#4200,#4198,#775,.T.);
#5347=EDGE_CURVE('',#4190,#4200,#839,.T.);
#5348=EDGE_CURVE('',#4201,#4186,#840,.F.);
#5349=EDGE_CURVE('',#4202,#4201,#841,.T.);
#5350=EDGE_CURVE('',#4195,#4202,#776,.T.);
#5351=EDGE_CURVE('',#4203,#4203,#777,.T.);
#5352=EDGE_CURVE('',#4204,#4205,#119,.T.);
#5353=EDGE_CURVE('',#4206,#4204,#2592,.T.);
#5354=EDGE_CURVE('',#4207,#4206,#120,.T.);
#5355=EDGE_CURVE('',#4205,#4207,#2593,.T.);
#5356=EDGE_CURVE('',#4208,#4204,#121,.T.);
#5357=EDGE_CURVE('',#4209,#4208,#2594,.T.);
#5358=EDGE_CURVE('',#4206,#4209,#122,.T.);
#5359=EDGE_CURVE('',#4210,#4211,#2595,.T.);
#5360=EDGE_CURVE('',#4212,#4210,#2596,.T.);
#5361=EDGE_CURVE('',#4213,#4212,#2597,.T.);
#5362=EDGE_CURVE('',#4211,#4213,#2598,.T.);
#5363=EDGE_CURVE('',#4214,#4210,#2599,.T.);
#5364=EDGE_CURVE('',#4215,#4214,#2600,.T.);
#5365=EDGE_CURVE('',#4212,#4215,#2601,.T.);
#5366=EDGE_CURVE('',#4216,#4217,#2602,.T.);
#5367=EDGE_CURVE('',#4218,#4216,#2603,.T.);
#5368=EDGE_CURVE('',#4219,#4218,#2604,.T.);
#5369=EDGE_CURVE('',#4217,#4219,#2605,.T.);
#5370=EDGE_CURVE('',#4220,#4216,#2606,.T.);
#5371=EDGE_CURVE('',#4221,#4220,#2607,.T.);
#5372=EDGE_CURVE('',#4218,#4221,#2608,.T.);
#5373=EDGE_CURVE('',#4222,#4223,#2609,.T.);
#5374=EDGE_CURVE('',#4224,#4222,#2610,.T.);
#5375=EDGE_CURVE('',#4225,#4224,#2611,.T.);
#5376=EDGE_CURVE('',#4223,#4225,#2612,.T.);
#5377=EDGE_CURVE('',#4226,#4222,#2613,.T.);
#5378=EDGE_CURVE('',#4227,#4226,#2614,.T.);
#5379=EDGE_CURVE('',#4224,#4227,#2615,.T.);
#5380=EDGE_CURVE('',#4228,#4229,#2616,.T.);
#5381=EDGE_CURVE('',#4230,#4228,#2617,.T.);
#5382=EDGE_CURVE('',#4231,#4230,#2618,.T.);
#5383=EDGE_CURVE('',#4229,#4231,#2619,.T.);
#5384=EDGE_CURVE('',#4232,#4228,#2620,.T.);
#5385=EDGE_CURVE('',#4233,#4232,#2621,.T.);
#5386=EDGE_CURVE('',#4230,#4233,#2622,.T.);
#5387=EDGE_CURVE('',#4234,#4235,#123,.T.);
#5388=EDGE_CURVE('',#4234,#4236,#2623,.T.);
#5389=EDGE_CURVE('',#4237,#4236,#124,.T.);
#5390=EDGE_CURVE('',#4235,#4237,#2624,.T.);
#5391=EDGE_CURVE('',#4238,#4234,#125,.T.);
#5392=EDGE_CURVE('',#4239,#4238,#2625,.T.);
#5393=EDGE_CURVE('',#4236,#4239,#126,.T.);
#5394=EDGE_CURVE('',#4240,#4241,#127,.T.);
#5395=EDGE_CURVE('',#4240,#4242,#2626,.T.);
#5396=EDGE_CURVE('',#4243,#4242,#128,.T.);
#5397=EDGE_CURVE('',#4241,#4243,#2627,.T.);
#5398=EDGE_CURVE('',#4244,#4240,#129,.T.);
#5399=EDGE_CURVE('',#4245,#4244,#2628,.T.);
#5400=EDGE_CURVE('',#4242,#4245,#130,.T.);
#5401=EDGE_CURVE('',#4246,#4247,#2629,.T.);
#5402=EDGE_CURVE('',#4248,#4246,#2630,.T.);
#5403=EDGE_CURVE('',#4249,#4248,#2631,.T.);
#5404=EDGE_CURVE('',#4247,#4249,#2632,.T.);
#5405=EDGE_CURVE('',#4250,#4246,#2633,.T.);
#5406=EDGE_CURVE('',#4251,#4250,#2634,.T.);
#5407=EDGE_CURVE('',#4248,#4251,#2635,.T.);
#5408=EDGE_CURVE('',#4252,#4253,#2636,.T.);
#5409=EDGE_CURVE('',#4254,#4252,#2637,.T.);
#5410=EDGE_CURVE('',#4255,#4254,#2638,.T.);
#5411=EDGE_CURVE('',#4253,#4255,#2639,.T.);
#5412=EDGE_CURVE('',#4256,#4252,#2640,.T.);
#5413=EDGE_CURVE('',#4257,#4256,#2641,.T.);
#5414=EDGE_CURVE('',#4254,#4257,#2642,.T.);
#5415=EDGE_CURVE('',#4258,#4259,#131,.T.);
#5416=EDGE_CURVE('',#4258,#4260,#2643,.T.);
#5417=EDGE_CURVE('',#4261,#4260,#132,.T.);
#5418=EDGE_CURVE('',#4259,#4261,#2644,.T.);
#5419=EDGE_CURVE('',#4262,#4258,#133,.T.);
#5420=EDGE_CURVE('',#4263,#4262,#2645,.T.);
#5421=EDGE_CURVE('',#4260,#4263,#134,.T.);
#5422=EDGE_CURVE('',#4264,#4265,#2646,.T.);
#5423=EDGE_CURVE('',#4266,#4264,#2647,.T.);
#5424=EDGE_CURVE('',#4267,#4266,#2648,.T.);
#5425=EDGE_CURVE('',#4265,#4267,#2649,.T.);
#5426=EDGE_CURVE('',#4268,#4264,#2650,.T.);
#5427=EDGE_CURVE('',#4269,#4268,#2651,.T.);
#5428=EDGE_CURVE('',#4266,#4269,#2652,.T.);
#5429=EDGE_CURVE('',#4270,#4271,#135,.T.);
#5430=EDGE_CURVE('',#4272,#4270,#2653,.T.);
#5431=EDGE_CURVE('',#4273,#4272,#136,.T.);
#5432=EDGE_CURVE('',#4271,#4273,#2654,.T.);
#5433=EDGE_CURVE('',#4274,#4270,#137,.T.);
#5434=EDGE_CURVE('',#4275,#4274,#2655,.T.);
#5435=EDGE_CURVE('',#4272,#4275,#138,.T.);
#5436=EDGE_CURVE('',#4276,#4277,#139,.T.);
#5437=EDGE_CURVE('',#4276,#4278,#2656,.T.);
#5438=EDGE_CURVE('',#4279,#4278,#140,.T.);
#5439=EDGE_CURVE('',#4277,#4279,#2657,.T.);
#5440=EDGE_CURVE('',#4280,#4276,#141,.T.);
#5441=EDGE_CURVE('',#4281,#4280,#2658,.T.);
#5442=EDGE_CURVE('',#4278,#4281,#142,.T.);
#5443=EDGE_CURVE('',#4239,#4282,#778,.T.);
#5444=EDGE_CURVE('',#4282,#4283,#2659,.T.);
#5445=EDGE_CURVE('',#4283,#4284,#779,.T.);
#5446=EDGE_CURVE('',#4261,#4284,#2660,.T.);
#5447=EDGE_CURVE('',#4263,#4243,#780,.T.);
#5448=EDGE_CURVE('',#4245,#4237,#781,.T.);
#5449=EDGE_CURVE('',#4211,#4285,#2661,.T.);
#5450=EDGE_CURVE('',#4285,#4286,#2662,.T.);
#5451=EDGE_CURVE('',#4286,#4283,#2663,.T.);
#5452=EDGE_CURVE('',#4282,#4250,#2664,.T.);
#5453=EDGE_CURVE('',#4247,#4232,#2665,.T.);
#5454=EDGE_CURVE('',#4229,#4256,#2666,.T.);
#5455=EDGE_CURVE('',#4253,#4226,#2667,.T.);
#5456=EDGE_CURVE('',#4223,#4220,#2668,.T.);
#5457=EDGE_CURVE('',#4217,#4268,#2669,.T.);
#5458=EDGE_CURVE('',#4265,#4214,#2670,.T.);
#5459=EDGE_CURVE('',#4277,#4207,#782,.T.);
#5460=EDGE_CURVE('',#4205,#4279,#783,.T.);
#5461=EDGE_CURVE('',#4287,#4213,#2671,.T.);
#5462=EDGE_CURVE('',#4275,#4287,#784,.T.);
#5463=EDGE_CURVE('',#4285,#4274,#785,.T.);
#5464=EDGE_CURVE('',#4269,#4219,#2672,.T.);
#5465=EDGE_CURVE('',#4257,#4231,#2673,.T.);
#5466=EDGE_CURVE('',#4241,#4262,#786,.T.);
#5467=EDGE_CURVE('',#4235,#4244,#787,.T.);
#5468=EDGE_CURVE('',#4288,#4238,#788,.T.);
#5469=EDGE_CURVE('',#4251,#4288,#2674,.T.);
#5470=EDGE_CURVE('',#4233,#4249,#2675,.T.);
#5471=EDGE_CURVE('',#4227,#4255,#2676,.T.);
#5472=EDGE_CURVE('',#4221,#4225,#2677,.T.);
#5473=EDGE_CURVE('',#4215,#4267,#2678,.T.);
#5474=EDGE_CURVE('',#4281,#4289,#2679,.T.);
#5475=EDGE_CURVE('',#4289,#4286,#789,.T.);
#5476=EDGE_CURVE('',#4271,#4208,#790,.T.);
#5477=EDGE_CURVE('',#4196,#4190,#2680,.T.);
#5478=EDGE_CURVE('',#4200,#4197,#2681,.T.);
#5479=EDGE_CURVE('',#4179,#4196,#2682,.T.);
#5480=EDGE_CURVE('',#4290,#4179,#2683,.T.);
#5481=EDGE_CURVE('',#4284,#4290,#2684,.T.);
#5482=EDGE_CURVE('',#4189,#4284,#2685,.T.);
#5483=EDGE_CURVE('',#4201,#4174,#2686,.T.);
#5484=EDGE_CURVE('',#4195,#4202,#2687,.T.);
#5485=EDGE_CURVE('',#4182,#4201,#2688,.T.);
#5486=EDGE_CURVE('',#4289,#4182,#2689,.T.);
#5487=EDGE_CURVE('',#4291,#4289,#2690,.T.);
#5488=EDGE_CURVE('',#4170,#4291,#2691,.T.);
#5489=EDGE_CURVE('',#4283,#4185,#2692,.T.);
#5490=EDGE_CURVE('',#4178,#4292,#2693,.T.);
#5491=EDGE_CURVE('',#4290,#4292,#791,.T.);
#5492=EDGE_CURVE('',#4293,#4291,#792,.T.);
#5493=EDGE_CURVE('',#4293,#4171,#2694,.T.);
#5494=EDGE_CURVE('',#4292,#4293,#2695,.T.);
#5495=EDGE_CURVE('',#4259,#4290,#2696,.T.);
#5496=EDGE_CURVE('',#4292,#4288,#2697,.T.);
#5497=EDGE_CURVE('',#4280,#4291,#2698,.T.);
#5498=EDGE_CURVE('',#4209,#4273,#793,.T.);
#5499=EDGE_CURVE('',#4287,#4293,#2699,.T.);
#5500=EDGE_CURVE('',#4181,#4286,#2700,.T.);
#5501=EDGE_CURVE('',#4203,#4294,#2701,.T.);
#5502=EDGE_CURVE('',#4294,#4294,#794,.T.);
#5503=EDGE_CURVE('',#4295,#4295,#795,.T.);
#5504=EDGE_CURVE('',#4199,#4295,#2702,.T.);
#5505=EDGE_CURVE('',#4296,#4297,#2703,.T.);
#5506=EDGE_CURVE('',#4296,#4298,#285,.T.);
#5507=EDGE_CURVE('',#4298,#4299,#796,.T.);
#5508=EDGE_CURVE('',#4299,#4297,#286,.T.);
#5509=EDGE_CURVE('',#4300,#4301,#2704,.T.);
#5510=EDGE_CURVE('',#4300,#4296,#287,.T.);
#5511=EDGE_CURVE('',#4297,#4301,#288,.T.);
#5512=EDGE_CURVE('',#4302,#4303,#2705,.T.);
#5513=EDGE_CURVE('',#4302,#4300,#289,.T.);
#5514=EDGE_CURVE('',#4301,#4303,#290,.T.);
#5515=EDGE_CURVE('',#4304,#4305,#2706,.T.);
#5516=EDGE_CURVE('',#4304,#4302,#291,.T.);
#5517=EDGE_CURVE('',#4303,#4305,#292,.T.);
#5518=EDGE_CURVE('',#4306,#4307,#2707,.T.);
#5519=EDGE_CURVE('',#4306,#4304,#293,.T.);
#5520=EDGE_CURVE('',#4305,#4307,#294,.T.);
#5521=EDGE_CURVE('',#4308,#4309,#2708,.T.);
#5522=EDGE_CURVE('',#4308,#4310,#295,.T.);
#5523=EDGE_CURVE('',#4309,#4310,#797,.T.);
#5524=EDGE_CURVE('',#4311,#4312,#2709,.T.);
#5525=EDGE_CURVE('',#4311,#4308,#296,.T.);
#5526=EDGE_CURVE('',#4313,#4309,#798,.T.);
#5527=EDGE_CURVE('',#4312,#4313,#297,.T.);
#5528=EDGE_CURVE('',#4314,#4315,#2710,.T.);
#5529=EDGE_CURVE('',#4314,#4311,#298,.T.);
#5530=EDGE_CURVE('',#4315,#4312,#299,.T.);
#5531=EDGE_CURVE('',#4316,#4317,#2711,.T.);
#5532=EDGE_CURVE('',#4316,#4314,#300,.T.);
#5533=EDGE_CURVE('',#4317,#4315,#301,.T.);
#5534=EDGE_CURVE('',#4318,#4319,#2712,.T.);
#5535=EDGE_CURVE('',#4318,#4316,#302,.T.);
#5536=EDGE_CURVE('',#4319,#4317,#303,.T.);
#5537=EDGE_CURVE('',#4310,#4320,#304,.T.);
#5538=EDGE_CURVE('',#4321,#4320,#799,.F.);
#5539=EDGE_CURVE('',#4322,#4321,#800,.F.);
#5540=EDGE_CURVE('',#4322,#4313,#305,.T.);
#5541=EDGE_CURVE('',#4307,#4322,#306,.T.);
#5542=EDGE_CURVE('',#4323,#4299,#307,.T.);
#5543=EDGE_CURVE('',#4323,#4319,#308,.T.);
#5544=EDGE_CURVE('',#4299,#4324,#801,.T.);
#5545=EDGE_CURVE('',#4324,#4298,#802,.T.);
#5546=EDGE_CURVE('',#4298,#4325,#309,.T.);
#5547=EDGE_CURVE('',#4325,#4323,#803,.T.);
#5548=EDGE_CURVE('',#4325,#4318,#310,.T.);
#5549=EDGE_CURVE('',#4320,#4306,#311,.T.);
#5550=EDGE_CURVE('',#4326,#4327,#2713,.T.);
#5551=EDGE_CURVE('',#4326,#4328,#2714,.T.);
#5552=EDGE_CURVE('',#4328,#4329,#2715,.T.);
#5553=EDGE_CURVE('',#4327,#4329,#2716,.T.);
#5554=EDGE_CURVE('',#4330,#4326,#2717,.T.);
#5555=EDGE_CURVE('',#4330,#4331,#2718,.T.);
#5556=EDGE_CURVE('',#4331,#4328,#2719,.T.);
#5557=EDGE_CURVE('',#4332,#4330,#2720,.T.);
#5558=EDGE_CURVE('',#4332,#4333,#2721,.T.);
#5559=EDGE_CURVE('',#4333,#4331,#2722,.T.);
#5560=EDGE_CURVE('',#4334,#4332,#2723,.T.);
#5561=EDGE_CURVE('',#4334,#4335,#2724,.T.);
#5562=EDGE_CURVE('',#4335,#4333,#2725,.T.);
#5563=EDGE_CURVE('',#4336,#4334,#2726,.T.);
#5564=EDGE_CURVE('',#4336,#4337,#2727,.T.);
#5565=EDGE_CURVE('',#4337,#4335,#2728,.T.);
#5566=EDGE_CURVE('',#4327,#4336,#2729,.T.);
#5567=EDGE_CURVE('',#4329,#4337,#2730,.T.);
#5568=EDGE_CURVE('',#4338,#4338,#804,.T.);
#5569=EDGE_CURVE('',#4324,#4338,#2731,.T.);
#5570=EDGE_CURVE('',#4320,#4322,#805,.F.);
#5571=EDGE_CURVE('',#4339,#4339,#806,.T.);
#5572=EDGE_CURVE('',#4339,#4321,#2732,.T.);
#5573=EDGE_CURVE('',#4340,#4341,#2733,.T.);
#5574=EDGE_CURVE('',#4340,#4342,#312,.T.);
#5575=EDGE_CURVE('',#4342,#4343,#807,.T.);
#5576=EDGE_CURVE('',#4343,#4341,#313,.T.);
#5577=EDGE_CURVE('',#4344,#4345,#2734,.T.);
#5578=EDGE_CURVE('',#4344,#4340,#314,.T.);
#5579=EDGE_CURVE('',#4341,#4345,#315,.T.);
#5580=EDGE_CURVE('',#4346,#4347,#2735,.T.);
#5581=EDGE_CURVE('',#4346,#4344,#316,.T.);
#5582=EDGE_CURVE('',#4345,#4347,#317,.T.);
#5583=EDGE_CURVE('',#4348,#4349,#2736,.T.);
#5584=EDGE_CURVE('',#4348,#4346,#318,.T.);
#5585=EDGE_CURVE('',#4347,#4349,#319,.T.);
#5586=EDGE_CURVE('',#4350,#4351,#2737,.T.);
#5587=EDGE_CURVE('',#4350,#4348,#320,.T.);
#5588=EDGE_CURVE('',#4349,#4351,#321,.T.);
#5589=EDGE_CURVE('',#4352,#4353,#2738,.T.);
#5590=EDGE_CURVE('',#4352,#4350,#322,.T.);
#5591=EDGE_CURVE('',#4351,#4353,#323,.T.);
#5592=EDGE_CURVE('',#4354,#4355,#2739,.T.);
#5593=EDGE_CURVE('',#4354,#4352,#324,.T.);
#5594=EDGE_CURVE('',#4353,#4355,#325,.T.);
#5595=EDGE_CURVE('',#4356,#4357,#2740,.T.);
#5596=EDGE_CURVE('',#4356,#4354,#326,.T.);
#5597=EDGE_CURVE('',#4355,#4357,#327,.T.);
#5598=EDGE_CURVE('',#4358,#4359,#2741,.T.);
#5599=EDGE_CURVE('',#4358,#4356,#328,.T.);
#5600=EDGE_CURVE('',#4357,#4359,#329,.T.);
#5601=EDGE_CURVE('',#4360,#4361,#2742,.T.);
#5602=EDGE_CURVE('',#4360,#4358,#330,.T.);
#5603=EDGE_CURVE('',#4359,#4361,#331,.T.);
#5604=EDGE_CURVE('',#4362,#4363,#2743,.T.);
#5605=EDGE_CURVE('',#4362,#4360,#332,.T.);
#5606=EDGE_CURVE('',#4361,#4363,#333,.T.);
#5607=EDGE_CURVE('',#4364,#4365,#2744,.T.);
#5608=EDGE_CURVE('',#4364,#4362,#334,.T.);
#5609=EDGE_CURVE('',#4363,#4365,#335,.T.);
#5610=EDGE_CURVE('',#4366,#4367,#2745,.T.);
#5611=EDGE_CURVE('',#4366,#4368,#336,.T.);
#5612=EDGE_CURVE('',#4369,#4368,#808,.T.);
#5613=EDGE_CURVE('',#4367,#4369,#337,.T.);
#5614=EDGE_CURVE('',#4370,#4371,#2746,.T.);
#5615=EDGE_CURVE('',#4370,#4366,#338,.T.);
#5616=EDGE_CURVE('',#4371,#4367,#339,.T.);
#5617=EDGE_CURVE('',#4372,#4373,#2747,.T.);
#5618=EDGE_CURVE('',#4372,#4370,#340,.T.);
#5619=EDGE_CURVE('',#4373,#4371,#341,.T.);
#5620=EDGE_CURVE('',#4374,#4375,#2748,.T.);
#5621=EDGE_CURVE('',#4374,#4372,#342,.T.);
#5622=EDGE_CURVE('',#4375,#4373,#343,.T.);
#5623=EDGE_CURVE('',#4376,#4377,#2749,.T.);
#5624=EDGE_CURVE('',#4376,#4374,#344,.T.);
#5625=EDGE_CURVE('',#4377,#4375,#345,.T.);
#5626=EDGE_CURVE('',#4378,#4379,#2750,.T.);
#5627=EDGE_CURVE('',#4378,#4376,#346,.T.);
#5628=EDGE_CURVE('',#4379,#4377,#347,.T.);
#5629=EDGE_CURVE('',#4380,#4381,#2751,.T.);
#5630=EDGE_CURVE('',#4380,#4378,#348,.T.);
#5631=EDGE_CURVE('',#4381,#4379,#349,.T.);
#5632=EDGE_CURVE('',#4382,#4383,#2752,.T.);
#5633=EDGE_CURVE('',#4382,#4380,#350,.T.);
#5634=EDGE_CURVE('',#4383,#4381,#351,.T.);
#5635=EDGE_CURVE('',#4384,#4385,#2753,.T.);
#5636=EDGE_CURVE('',#4384,#4382,#352,.T.);
#5637=EDGE_CURVE('',#4385,#4383,#353,.T.);
#5638=EDGE_CURVE('',#4386,#4387,#2754,.T.);
#5639=EDGE_CURVE('',#4386,#4384,#354,.T.);
#5640=EDGE_CURVE('',#4387,#4385,#355,.T.);
#5641=EDGE_CURVE('',#4388,#4389,#2755,.T.);
#5642=EDGE_CURVE('',#4388,#4386,#356,.T.);
#5643=EDGE_CURVE('',#4389,#4387,#357,.T.);
#5644=EDGE_CURVE('',#4390,#4391,#2756,.T.);
#5645=EDGE_CURVE('',#4390,#4388,#358,.T.);
#5646=EDGE_CURVE('',#4391,#4389,#359,.T.);
#5647=EDGE_CURVE('',#4368,#4392,#360,.T.);
#5648=EDGE_CURVE('',#4393,#4392,#809,.T.);
#5649=EDGE_CURVE('',#4394,#4393,#810,.T.);
#5650=EDGE_CURVE('',#4394,#4369,#361,.T.);
#5651=EDGE_CURVE('',#4365,#4394,#362,.T.);
#5652=EDGE_CURVE('',#4395,#4343,#363,.T.);
#5653=EDGE_CURVE('',#4395,#4391,#364,.T.);
#5654=EDGE_CURVE('',#4343,#4396,#811,.T.);
#5655=EDGE_CURVE('',#4396,#4342,#812,.T.);
#5656=EDGE_CURVE('',#4342,#4397,#365,.T.);
#5657=EDGE_CURVE('',#4397,#4395,#813,.T.);
#5658=EDGE_CURVE('',#4397,#4390,#366,.T.);
#5659=EDGE_CURVE('',#4392,#4364,#367,.T.);
#5660=EDGE_CURVE('',#4398,#4399,#2757,.T.);
#5661=EDGE_CURVE('',#4399,#4399,#814,.T.);
#5662=EDGE_CURVE('',#4400,#4401,#2758,.T.);
#5663=EDGE_CURVE('',#4400,#4402,#2759,.T.);
#5664=EDGE_CURVE('',#4402,#4403,#2760,.T.);
#5665=EDGE_CURVE('',#4401,#4403,#2761,.T.);
#5666=EDGE_CURVE('',#4404,#4400,#2762,.T.);
#5667=EDGE_CURVE('',#4404,#4405,#2763,.T.);
#5668=EDGE_CURVE('',#4405,#4402,#2764,.T.);
#5669=EDGE_CURVE('',#4406,#4404,#2765,.T.);
#5670=EDGE_CURVE('',#4406,#4407,#2766,.T.);
#5671=EDGE_CURVE('',#4407,#4405,#2767,.T.);
#5672=EDGE_CURVE('',#4408,#4406,#2768,.T.);
#5673=EDGE_CURVE('',#4408,#4409,#2769,.T.);
#5674=EDGE_CURVE('',#4409,#4407,#2770,.T.);
#5675=EDGE_CURVE('',#4410,#4408,#2771,.T.);
#5676=EDGE_CURVE('',#4410,#4411,#2772,.T.);
#5677=EDGE_CURVE('',#4411,#4409,#2773,.T.);
#5678=EDGE_CURVE('',#4401,#4410,#2774,.T.);
#5679=EDGE_CURVE('',#4403,#4411,#2775,.T.);
#5680=EDGE_CURVE('',#4412,#4412,#815,.T.);
#5681=EDGE_CURVE('',#4396,#4412,#2776,.T.);
#5682=EDGE_CURVE('',#4392,#4394,#816,.T.);
#5683=EDGE_CURVE('',#4413,#4413,#817,.T.);
#5684=EDGE_CURVE('',#4413,#4393,#2777,.T.);
#5685=EDGE_CURVE('',#4414,#4414,#818,.T.);
#5686=EDGE_CURVE('',#4415,#4415,#819,.T.);
#5687=EDGE_CURVE('',#4415,#4414,#2778,.T.);
#5688=EDGE_CURVE('',#4416,#4416,#820,.T.);
#5689=EDGE_CURVE('',#4416,#4415,#2779,.T.);
#5690=EDGE_CURVE('',#4417,#4417,#821,.T.);
#5691=EDGE_CURVE('',#4417,#4416,#2780,.T.);
#5692=ORIENTED_EDGE('',*,*,#4418,.F.);
#5693=ORIENTED_EDGE('',*,*,#4419,.F.);
#5694=ORIENTED_EDGE('',*,*,#4420,.F.);
#5695=ORIENTED_EDGE('',*,*,#4421,.F.);
#5696=ORIENTED_EDGE('',*,*,#4422,.F.);
#5697=ORIENTED_EDGE('',*,*,#4423,.F.);
#5698=ORIENTED_EDGE('',*,*,#4424,.F.);
#5699=ORIENTED_EDGE('',*,*,#4425,.F.);
#5700=ORIENTED_EDGE('',*,*,#4426,.F.);
#5701=ORIENTED_EDGE('',*,*,#4427,.F.);
#5702=ORIENTED_EDGE('',*,*,#4428,.F.);
#5703=ORIENTED_EDGE('',*,*,#4429,.F.);
#5704=ORIENTED_EDGE('',*,*,#4430,.T.);
#5705=ORIENTED_EDGE('',*,*,#4431,.T.);
#5706=ORIENTED_EDGE('',*,*,#4428,.T.);
#5707=ORIENTED_EDGE('',*,*,#4432,.T.);
#5708=ORIENTED_EDGE('',*,*,#4422,.T.);
#5709=ORIENTED_EDGE('',*,*,#4433,.T.);
#5710=ORIENTED_EDGE('',*,*,#4429,.T.);
#5711=ORIENTED_EDGE('',*,*,#4434,.T.);
#5712=ORIENTED_EDGE('',*,*,#4425,.T.);
#5713=ORIENTED_EDGE('',*,*,#4435,.T.);
#5714=ORIENTED_EDGE('',*,*,#4427,.T.);
#5715=ORIENTED_EDGE('',*,*,#4436,.T.);
#5716=ORIENTED_EDGE('',*,*,#4418,.T.);
#5717=ORIENTED_EDGE('',*,*,#4437,.T.);
#5718=ORIENTED_EDGE('',*,*,#4426,.T.);
#5719=ORIENTED_EDGE('',*,*,#4438,.T.);
#5720=ORIENTED_EDGE('',*,*,#4439,.T.);
#5721=ORIENTED_EDGE('',*,*,#4440,.T.);
#5722=ORIENTED_EDGE('',*,*,#4424,.T.);
#5723=ORIENTED_EDGE('',*,*,#4441,.T.);
#5724=ORIENTED_EDGE('',*,*,#4442,.T.);
#5725=ORIENTED_EDGE('',*,*,#4443,.T.);
#5726=ORIENTED_EDGE('',*,*,#4423,.T.);
#5727=ORIENTED_EDGE('',*,*,#4444,.T.);
#5728=ORIENTED_EDGE('',*,*,#4419,.T.);
#5729=ORIENTED_EDGE('',*,*,#4445,.T.);
#5730=ORIENTED_EDGE('',*,*,#4421,.T.);
#5731=ORIENTED_EDGE('',*,*,#4446,.T.);
#5732=ORIENTED_EDGE('',*,*,#4447,.T.);
#5733=ORIENTED_EDGE('',*,*,#4448,.T.);
#5734=ORIENTED_EDGE('',*,*,#4420,.T.);
#5735=ORIENTED_EDGE('',*,*,#4449,.T.);
#5736=ORIENTED_EDGE('',*,*,#4432,.F.);
#5737=ORIENTED_EDGE('',*,*,#4435,.F.);
#5738=ORIENTED_EDGE('',*,*,#4440,.F.);
#5739=ORIENTED_EDGE('',*,*,#4450,.T.);
#5740=ORIENTED_EDGE('',*,*,#4451,.T.);
#5741=ORIENTED_EDGE('',*,*,#4452,.T.);
#5742=ORIENTED_EDGE('',*,*,#4453,.T.);
#5743=ORIENTED_EDGE('',*,*,#4441,.F.);
#5744=ORIENTED_EDGE('',*,*,#4437,.F.);
#5745=ORIENTED_EDGE('',*,*,#4448,.F.);
#5746=ORIENTED_EDGE('',*,*,#4454,.T.);
#5747=ORIENTED_EDGE('',*,*,#4433,.F.);
#5748=ORIENTED_EDGE('',*,*,#4445,.F.);
#5749=ORIENTED_EDGE('',*,*,#4438,.F.);
#5750=ORIENTED_EDGE('',*,*,#4436,.F.);
#5751=ORIENTED_EDGE('',*,*,#4455,.F.);
#5752=ORIENTED_EDGE('',*,*,#4456,.T.);
#5753=ORIENTED_EDGE('',*,*,#4453,.F.);
#5754=ORIENTED_EDGE('',*,*,#4456,.F.);
#5755=ORIENTED_EDGE('',*,*,#4457,.F.);
#5756=ORIENTED_EDGE('',*,*,#4458,.T.);
#5757=ORIENTED_EDGE('',*,*,#4452,.F.);
#5758=ORIENTED_EDGE('',*,*,#4458,.F.);
#5759=ORIENTED_EDGE('',*,*,#4459,.F.);
#5760=ORIENTED_EDGE('',*,*,#4460,.T.);
#5761=ORIENTED_EDGE('',*,*,#4451,.F.);
#5762=ORIENTED_EDGE('',*,*,#4460,.F.);
#5763=ORIENTED_EDGE('',*,*,#4430,.F.);
#5764=ORIENTED_EDGE('',*,*,#4450,.F.);
#5765=ORIENTED_EDGE('',*,*,#4439,.F.);
#5766=ORIENTED_EDGE('',*,*,#4454,.F.);
#5767=ORIENTED_EDGE('',*,*,#4447,.F.);
#5768=ORIENTED_EDGE('',*,*,#4461,.F.);
#5769=ORIENTED_EDGE('',*,*,#4442,.F.);
#5770=ORIENTED_EDGE('',*,*,#4462,.F.);
#5771=ORIENTED_EDGE('',*,*,#4431,.F.);
#5772=ORIENTED_EDGE('',*,*,#4462,.T.);
#5773=ORIENTED_EDGE('',*,*,#4444,.F.);
#5774=ORIENTED_EDGE('',*,*,#4434,.F.);
#5775=ORIENTED_EDGE('',*,*,#4443,.F.);
#5776=ORIENTED_EDGE('',*,*,#4461,.T.);
#5777=ORIENTED_EDGE('',*,*,#4449,.F.);
#5778=ORIENTED_EDGE('',*,*,#4446,.F.);
#5779=ORIENTED_EDGE('',*,*,#4455,.T.);
#5780=ORIENTED_EDGE('',*,*,#4457,.T.);
#5781=ORIENTED_EDGE('',*,*,#4459,.T.);
#5782=ORIENTED_EDGE('',*,*,#4463,.F.);
#5783=ORIENTED_EDGE('',*,*,#4464,.F.);
#5784=ORIENTED_EDGE('',*,*,#4465,.F.);
#5785=ORIENTED_EDGE('',*,*,#4466,.F.);
#5786=ORIENTED_EDGE('',*,*,#4467,.F.);
#5787=ORIENTED_EDGE('',*,*,#4468,.F.);
#5788=ORIENTED_EDGE('',*,*,#4469,.T.);
#5789=ORIENTED_EDGE('',*,*,#4470,.T.);
#5790=ORIENTED_EDGE('',*,*,#4467,.T.);
#5791=ORIENTED_EDGE('',*,*,#4471,.T.);
#5792=ORIENTED_EDGE('',*,*,#4464,.T.);
#5793=ORIENTED_EDGE('',*,*,#4472,.T.);
#5794=ORIENTED_EDGE('',*,*,#4468,.T.);
#5795=ORIENTED_EDGE('',*,*,#4473,.T.);
#5796=ORIENTED_EDGE('',*,*,#4474,.F.);
#5797=ORIENTED_EDGE('',*,*,#4475,.F.);
#5798=ORIENTED_EDGE('',*,*,#4476,.F.);
#5799=ORIENTED_EDGE('',*,*,#4477,.F.);
#5800=ORIENTED_EDGE('',*,*,#4478,.F.);
#5801=ORIENTED_EDGE('',*,*,#4479,.F.);
#5802=ORIENTED_EDGE('',*,*,#4480,.T.);
#5803=ORIENTED_EDGE('',*,*,#4481,.T.);
#5804=ORIENTED_EDGE('',*,*,#4478,.T.);
#5805=ORIENTED_EDGE('',*,*,#4482,.T.);
#5806=ORIENTED_EDGE('',*,*,#4466,.T.);
#5807=ORIENTED_EDGE('',*,*,#4483,.T.);
#5808=ORIENTED_EDGE('',*,*,#4479,.T.);
#5809=ORIENTED_EDGE('',*,*,#4484,.T.);
#5810=ORIENTED_EDGE('',*,*,#4475,.T.);
#5811=ORIENTED_EDGE('',*,*,#4485,.T.);
#5812=ORIENTED_EDGE('',*,*,#4477,.T.);
#5813=ORIENTED_EDGE('',*,*,#4486,.T.);
#5814=ORIENTED_EDGE('',*,*,#4463,.T.);
#5815=ORIENTED_EDGE('',*,*,#4487,.T.);
#5816=ORIENTED_EDGE('',*,*,#4476,.T.);
#5817=ORIENTED_EDGE('',*,*,#4488,.T.);
#5818=ORIENTED_EDGE('',*,*,#4489,.T.);
#5819=ORIENTED_EDGE('',*,*,#4490,.T.);
#5820=ORIENTED_EDGE('',*,*,#4474,.T.);
#5821=ORIENTED_EDGE('',*,*,#4491,.T.);
#5822=ORIENTED_EDGE('',*,*,#4492,.T.);
#5823=ORIENTED_EDGE('',*,*,#4493,.T.);
#5824=ORIENTED_EDGE('',*,*,#4465,.T.);
#5825=ORIENTED_EDGE('',*,*,#4494,.T.);
#5826=ORIENTED_EDGE('',*,*,#4482,.F.);
#5827=ORIENTED_EDGE('',*,*,#4485,.F.);
#5828=ORIENTED_EDGE('',*,*,#4490,.F.);
#5829=ORIENTED_EDGE('',*,*,#4495,.T.);
#5830=ORIENTED_EDGE('',*,*,#4491,.F.);
#5831=ORIENTED_EDGE('',*,*,#4487,.F.);
#5832=ORIENTED_EDGE('',*,*,#4493,.F.);
#5833=ORIENTED_EDGE('',*,*,#4496,.T.);
#5834=ORIENTED_EDGE('',*,*,#4472,.F.);
#5835=ORIENTED_EDGE('',*,*,#4488,.F.);
#5836=ORIENTED_EDGE('',*,*,#4486,.F.);
#5837=ORIENTED_EDGE('',*,*,#4483,.F.);
#5838=ORIENTED_EDGE('',*,*,#4480,.F.);
#5839=ORIENTED_EDGE('',*,*,#4495,.F.);
#5840=ORIENTED_EDGE('',*,*,#4489,.F.);
#5841=ORIENTED_EDGE('',*,*,#4496,.F.);
#5842=ORIENTED_EDGE('',*,*,#4492,.F.);
#5843=ORIENTED_EDGE('',*,*,#4497,.F.);
#5844=ORIENTED_EDGE('',*,*,#4469,.F.);
#5845=ORIENTED_EDGE('',*,*,#4498,.F.);
#5846=ORIENTED_EDGE('',*,*,#4481,.F.);
#5847=ORIENTED_EDGE('',*,*,#4498,.T.);
#5848=ORIENTED_EDGE('',*,*,#4471,.F.);
#5849=ORIENTED_EDGE('',*,*,#4484,.F.);
#5850=ORIENTED_EDGE('',*,*,#4470,.F.);
#5851=ORIENTED_EDGE('',*,*,#4497,.T.);
#5852=ORIENTED_EDGE('',*,*,#4494,.F.);
#5853=ORIENTED_EDGE('',*,*,#4473,.F.);
#5854=ORIENTED_EDGE('',*,*,#4499,.T.);
#5855=ORIENTED_EDGE('',*,*,#4500,.T.);
#5856=ORIENTED_EDGE('',*,*,#4501,.T.);
#5857=ORIENTED_EDGE('',*,*,#4502,.T.);
#5858=ORIENTED_EDGE('',*,*,#4499,.F.);
#5859=ORIENTED_EDGE('',*,*,#4503,.T.);
#5860=ORIENTED_EDGE('',*,*,#4504,.T.);
#5861=ORIENTED_EDGE('',*,*,#4505,.T.);
#5862=ORIENTED_EDGE('',*,*,#4506,.T.);
#5863=ORIENTED_EDGE('',*,*,#4507,.T.);
#5864=ORIENTED_EDGE('',*,*,#4504,.F.);
#5865=ORIENTED_EDGE('',*,*,#4508,.T.);
#5866=ORIENTED_EDGE('',*,*,#4506,.F.);
#5867=ORIENTED_EDGE('',*,*,#4509,.T.);
#5868=ORIENTED_EDGE('',*,*,#4510,.T.);
#5869=ORIENTED_EDGE('',*,*,#4511,.T.);
#5870=ORIENTED_EDGE('',*,*,#4512,.T.);
#5871=ORIENTED_EDGE('',*,*,#4513,.T.);
#5872=ORIENTED_EDGE('',*,*,#4510,.F.);
#5873=ORIENTED_EDGE('',*,*,#4514,.T.);
#5874=ORIENTED_EDGE('',*,*,#4512,.F.);
#5875=ORIENTED_EDGE('',*,*,#4515,.T.);
#5876=ORIENTED_EDGE('',*,*,#4516,.T.);
#5877=ORIENTED_EDGE('',*,*,#4517,.T.);
#5878=ORIENTED_EDGE('',*,*,#4518,.T.);
#5879=ORIENTED_EDGE('',*,*,#4519,.T.);
#5880=ORIENTED_EDGE('',*,*,#4516,.F.);
#5881=ORIENTED_EDGE('',*,*,#4520,.T.);
#5882=ORIENTED_EDGE('',*,*,#4518,.F.);
#5883=ORIENTED_EDGE('',*,*,#4521,.T.);
#5884=ORIENTED_EDGE('',*,*,#4501,.F.);
#5885=ORIENTED_EDGE('',*,*,#4522,.T.);
#5886=ORIENTED_EDGE('',*,*,#4509,.F.);
#5887=ORIENTED_EDGE('',*,*,#4523,.T.);
#5888=ORIENTED_EDGE('',*,*,#4524,.F.);
#5889=ORIENTED_EDGE('',*,*,#4525,.T.);
#5890=ORIENTED_EDGE('',*,*,#4508,.F.);
#5891=ORIENTED_EDGE('',*,*,#4526,.F.);
#5892=ORIENTED_EDGE('',*,*,#4527,.F.);
#5893=ORIENTED_EDGE('',*,*,#4523,.F.);
#5894=ORIENTED_EDGE('',*,*,#4503,.F.);
#5895=ORIENTED_EDGE('',*,*,#4528,.T.);
#5896=ORIENTED_EDGE('',*,*,#4529,.F.);
#5897=ORIENTED_EDGE('',*,*,#4526,.T.);
#5898=ORIENTED_EDGE('',*,*,#4502,.F.);
#5899=ORIENTED_EDGE('',*,*,#4530,.F.);
#5900=ORIENTED_EDGE('',*,*,#4531,.F.);
#5901=ORIENTED_EDGE('',*,*,#4528,.F.);
#5902=ORIENTED_EDGE('',*,*,#4500,.F.);
#5903=ORIENTED_EDGE('',*,*,#4505,.F.);
#5904=ORIENTED_EDGE('',*,*,#4507,.F.);
#5905=ORIENTED_EDGE('',*,*,#4511,.F.);
#5906=ORIENTED_EDGE('',*,*,#4513,.F.);
#5907=ORIENTED_EDGE('',*,*,#4517,.F.);
#5908=ORIENTED_EDGE('',*,*,#4519,.F.);
#5909=ORIENTED_EDGE('',*,*,#4522,.F.);
#5910=ORIENTED_EDGE('',*,*,#4532,.T.);
#5911=ORIENTED_EDGE('',*,*,#4533,.T.);
#5912=ORIENTED_EDGE('',*,*,#4534,.T.);
#5913=ORIENTED_EDGE('',*,*,#4535,.T.);
#5914=ORIENTED_EDGE('',*,*,#4536,.T.);
#5915=ORIENTED_EDGE('',*,*,#4537,.T.);
#5916=ORIENTED_EDGE('',*,*,#4538,.T.);
#5917=ORIENTED_EDGE('',*,*,#4539,.T.);
#5918=ORIENTED_EDGE('',*,*,#4540,.T.);
#5919=ORIENTED_EDGE('',*,*,#4541,.T.);
#5920=ORIENTED_EDGE('',*,*,#4542,.T.);
#5921=ORIENTED_EDGE('',*,*,#4537,.F.);
#5922=ORIENTED_EDGE('',*,*,#4524,.T.);
#5923=ORIENTED_EDGE('',*,*,#4543,.T.);
#5924=ORIENTED_EDGE('',*,*,#4544,.T.);
#5925=ORIENTED_EDGE('',*,*,#4541,.F.);
#5926=ORIENTED_EDGE('',*,*,#4527,.T.);
#5927=ORIENTED_EDGE('',*,*,#4545,.T.);
#5928=ORIENTED_EDGE('',*,*,#4546,.T.);
#5929=ORIENTED_EDGE('',*,*,#4543,.F.);
#5930=ORIENTED_EDGE('',*,*,#4529,.T.);
#5931=ORIENTED_EDGE('',*,*,#4547,.T.);
#5932=ORIENTED_EDGE('',*,*,#4548,.T.);
#5933=ORIENTED_EDGE('',*,*,#4545,.F.);
#5934=ORIENTED_EDGE('',*,*,#4531,.T.);
#5935=ORIENTED_EDGE('',*,*,#4549,.T.);
#5936=ORIENTED_EDGE('',*,*,#4550,.T.);
#5937=ORIENTED_EDGE('',*,*,#4547,.F.);
#5938=ORIENTED_EDGE('',*,*,#4551,.T.);
#5939=ORIENTED_EDGE('',*,*,#4552,.T.);
#5940=ORIENTED_EDGE('',*,*,#4553,.T.);
#5941=ORIENTED_EDGE('',*,*,#4549,.F.);
#5942=ORIENTED_EDGE('',*,*,#4554,.T.);
#5943=ORIENTED_EDGE('',*,*,#4555,.T.);
#5944=ORIENTED_EDGE('',*,*,#4556,.T.);
#5945=ORIENTED_EDGE('',*,*,#4557,.T.);
#5946=ORIENTED_EDGE('',*,*,#4558,.T.);
#5947=ORIENTED_EDGE('',*,*,#4539,.F.);
#5948=ORIENTED_EDGE('',*,*,#4559,.T.);
#5949=ORIENTED_EDGE('',*,*,#4555,.F.);
#5950=ORIENTED_EDGE('',*,*,#4560,.T.);
#5951=ORIENTED_EDGE('',*,*,#4514,.F.);
#5952=ORIENTED_EDGE('',*,*,#4525,.F.);
#5953=ORIENTED_EDGE('',*,*,#4540,.F.);
#5954=ORIENTED_EDGE('',*,*,#4561,.F.);
#5955=ORIENTED_EDGE('',*,*,#4546,.F.);
#5956=ORIENTED_EDGE('',*,*,#4562,.F.);
#5957=ORIENTED_EDGE('',*,*,#4563,.F.);
#5958=ORIENTED_EDGE('',*,*,#4564,.T.);
#5959=ORIENTED_EDGE('',*,*,#4548,.F.);
#5960=ORIENTED_EDGE('',*,*,#4565,.F.);
#5961=ORIENTED_EDGE('',*,*,#4566,.F.);
#5962=ORIENTED_EDGE('',*,*,#4562,.T.);
#5963=ORIENTED_EDGE('',*,*,#4550,.F.);
#5964=ORIENTED_EDGE('',*,*,#4567,.F.);
#5965=ORIENTED_EDGE('',*,*,#4568,.F.);
#5966=ORIENTED_EDGE('',*,*,#4565,.T.);
#5967=ORIENTED_EDGE('',*,*,#4556,.F.);
#5968=ORIENTED_EDGE('',*,*,#4569,.F.);
#5969=ORIENTED_EDGE('',*,*,#4570,.F.);
#5970=ORIENTED_EDGE('',*,*,#4571,.T.);
#5971=ORIENTED_EDGE('',*,*,#4572,.T.);
#5972=ORIENTED_EDGE('',*,*,#4573,.T.);
#5973=ORIENTED_EDGE('',*,*,#4574,.F.);
#5974=ORIENTED_EDGE('',*,*,#4575,.T.);
#5975=ORIENTED_EDGE('',*,*,#4576,.T.);
#5976=ORIENTED_EDGE('',*,*,#4577,.T.);
#5977=ORIENTED_EDGE('',*,*,#4578,.T.);
#5978=ORIENTED_EDGE('',*,*,#4579,.T.);
#5979=ORIENTED_EDGE('',*,*,#4580,.F.);
#5980=ORIENTED_EDGE('',*,*,#4553,.F.);
#5981=ORIENTED_EDGE('',*,*,#4581,.F.);
#5982=ORIENTED_EDGE('',*,*,#4582,.T.);
#5983=ORIENTED_EDGE('',*,*,#4583,.F.);
#5984=ORIENTED_EDGE('',*,*,#4567,.T.);
#5985=ORIENTED_EDGE('',*,*,#4552,.F.);
#5986=ORIENTED_EDGE('',*,*,#4584,.F.);
#5987=ORIENTED_EDGE('',*,*,#4585,.T.);
#5988=ORIENTED_EDGE('',*,*,#4586,.F.);
#5989=ORIENTED_EDGE('',*,*,#4587,.F.);
#5990=ORIENTED_EDGE('',*,*,#4588,.F.);
#5991=ORIENTED_EDGE('',*,*,#4582,.F.);
#5992=ORIENTED_EDGE('',*,*,#4581,.T.);
#5993=ORIENTED_EDGE('',*,*,#4558,.F.);
#5994=ORIENTED_EDGE('',*,*,#4589,.T.);
#5995=ORIENTED_EDGE('',*,*,#4590,.T.);
#5996=ORIENTED_EDGE('',*,*,#4584,.T.);
#5997=ORIENTED_EDGE('',*,*,#4591,.T.);
#5998=ORIENTED_EDGE('',*,*,#4592,.T.);
#5999=ORIENTED_EDGE('',*,*,#4593,.T.);
#6000=ORIENTED_EDGE('',*,*,#4594,.T.);
#6001=ORIENTED_EDGE('',*,*,#4595,.T.);
#6002=ORIENTED_EDGE('',*,*,#4596,.T.);
#6003=ORIENTED_EDGE('',*,*,#4597,.T.);
#6004=ORIENTED_EDGE('',*,*,#4592,.F.);
#6005=ORIENTED_EDGE('',*,*,#4595,.F.);
#6006=ORIENTED_EDGE('',*,*,#4598,.T.);
#6007=ORIENTED_EDGE('',*,*,#4599,.T.);
#6008=ORIENTED_EDGE('',*,*,#4600,.F.);
#6009=ORIENTED_EDGE('',*,*,#4594,.F.);
#6010=ORIENTED_EDGE('',*,*,#4601,.T.);
#6011=ORIENTED_EDGE('',*,*,#4602,.T.);
#6012=ORIENTED_EDGE('',*,*,#4603,.T.);
#6013=ORIENTED_EDGE('',*,*,#4604,.T.);
#6014=ORIENTED_EDGE('',*,*,#4570,.T.);
#6015=ORIENTED_EDGE('',*,*,#4598,.F.);
#6016=ORIENTED_EDGE('',*,*,#4591,.F.);
#6017=ORIENTED_EDGE('',*,*,#4605,.T.);
#6018=ORIENTED_EDGE('',*,*,#4606,.T.);
#6019=ORIENTED_EDGE('',*,*,#4605,.F.);
#6020=ORIENTED_EDGE('',*,*,#4607,.T.);
#6021=ORIENTED_EDGE('',*,*,#4608,.T.);
#6022=ORIENTED_EDGE('',*,*,#4609,.T.);
#6023=ORIENTED_EDGE('',*,*,#4610,.T.);
#6024=ORIENTED_EDGE('',*,*,#4611,.T.);
#6025=ORIENTED_EDGE('',*,*,#4612,.T.);
#6026=ORIENTED_EDGE('',*,*,#4613,.T.);
#6027=ORIENTED_EDGE('',*,*,#4608,.F.);
#6028=ORIENTED_EDGE('',*,*,#4611,.F.);
#6029=ORIENTED_EDGE('',*,*,#4614,.T.);
#6030=ORIENTED_EDGE('',*,*,#4568,.T.);
#6031=ORIENTED_EDGE('',*,*,#4615,.F.);
#6032=ORIENTED_EDGE('',*,*,#4610,.F.);
#6033=ORIENTED_EDGE('',*,*,#4616,.T.);
#6034=ORIENTED_EDGE('',*,*,#4617,.F.);
#6035=ORIENTED_EDGE('',*,*,#4618,.T.);
#6036=ORIENTED_EDGE('',*,*,#4566,.T.);
#6037=ORIENTED_EDGE('',*,*,#4614,.F.);
#6038=ORIENTED_EDGE('',*,*,#4607,.F.);
#6039=ORIENTED_EDGE('',*,*,#4619,.T.);
#6040=ORIENTED_EDGE('',*,*,#4620,.T.);
#6041=ORIENTED_EDGE('',*,*,#4619,.F.);
#6042=ORIENTED_EDGE('',*,*,#4621,.T.);
#6043=ORIENTED_EDGE('',*,*,#4622,.T.);
#6044=ORIENTED_EDGE('',*,*,#4623,.T.);
#6045=ORIENTED_EDGE('',*,*,#4624,.T.);
#6046=ORIENTED_EDGE('',*,*,#4625,.T.);
#6047=ORIENTED_EDGE('',*,*,#4626,.T.);
#6048=ORIENTED_EDGE('',*,*,#4627,.T.);
#6049=ORIENTED_EDGE('',*,*,#4622,.F.);
#6050=ORIENTED_EDGE('',*,*,#4596,.F.);
#6051=ORIENTED_EDGE('',*,*,#4600,.T.);
#6052=ORIENTED_EDGE('',*,*,#4628,.T.);
#6053=ORIENTED_EDGE('',*,*,#4629,.F.);
#6054=ORIENTED_EDGE('',*,*,#4625,.F.);
#6055=ORIENTED_EDGE('',*,*,#4630,.T.);
#6056=ORIENTED_EDGE('',*,*,#4597,.F.);
#6057=ORIENTED_EDGE('',*,*,#4630,.F.);
#6058=ORIENTED_EDGE('',*,*,#4624,.F.);
#6059=ORIENTED_EDGE('',*,*,#4631,.F.);
#6060=ORIENTED_EDGE('',*,*,#4632,.F.);
#6061=ORIENTED_EDGE('',*,*,#4616,.F.);
#6062=ORIENTED_EDGE('',*,*,#4609,.F.);
#6063=ORIENTED_EDGE('',*,*,#4613,.F.);
#6064=ORIENTED_EDGE('',*,*,#4633,.F.);
#6065=ORIENTED_EDGE('',*,*,#4587,.T.);
#6066=ORIENTED_EDGE('',*,*,#4634,.T.);
#6067=ORIENTED_EDGE('',*,*,#4635,.T.);
#6068=ORIENTED_EDGE('',*,*,#4636,.T.);
#6069=ORIENTED_EDGE('',*,*,#4637,.T.);
#6070=ORIENTED_EDGE('',*,*,#4638,.T.);
#6071=ORIENTED_EDGE('',*,*,#4639,.T.);
#6072=ORIENTED_EDGE('',*,*,#4578,.F.);
#6073=ORIENTED_EDGE('',*,*,#4640,.T.);
#6074=ORIENTED_EDGE('',*,*,#4641,.T.);
#6075=ORIENTED_EDGE('',*,*,#4642,.T.);
#6076=ORIENTED_EDGE('',*,*,#4643,.T.);
#6077=ORIENTED_EDGE('',*,*,#4644,.T.);
#6078=ORIENTED_EDGE('',*,*,#4645,.T.);
#6079=ORIENTED_EDGE('',*,*,#4646,.T.);
#6080=ORIENTED_EDGE('',*,*,#4647,.F.);
#6081=ORIENTED_EDGE('',*,*,#4648,.T.);
#6082=ORIENTED_EDGE('',*,*,#4649,.T.);
#6083=ORIENTED_EDGE('',*,*,#4650,.T.);
#6084=ORIENTED_EDGE('',*,*,#4651,.T.);
#6085=ORIENTED_EDGE('',*,*,#4652,.T.);
#6086=ORIENTED_EDGE('',*,*,#4653,.T.);
#6087=ORIENTED_EDGE('',*,*,#4654,.T.);
#6088=ORIENTED_EDGE('',*,*,#4601,.F.);
#6089=ORIENTED_EDGE('',*,*,#4593,.F.);
#6090=ORIENTED_EDGE('',*,*,#4655,.T.);
#6091=ORIENTED_EDGE('',*,*,#4656,.T.);
#6092=ORIENTED_EDGE('',*,*,#4657,.T.);
#6093=ORIENTED_EDGE('',*,*,#4658,.T.);
#6094=ORIENTED_EDGE('',*,*,#4659,.T.);
#6095=ORIENTED_EDGE('',*,*,#4660,.T.);
#6096=ORIENTED_EDGE('',*,*,#4661,.T.);
#6097=ORIENTED_EDGE('',*,*,#4662,.T.);
#6098=ORIENTED_EDGE('',*,*,#4663,.T.);
#6099=ORIENTED_EDGE('',*,*,#4664,.T.);
#6100=ORIENTED_EDGE('',*,*,#4665,.T.);
#6101=ORIENTED_EDGE('',*,*,#4666,.T.);
#6102=ORIENTED_EDGE('',*,*,#4667,.T.);
#6103=ORIENTED_EDGE('',*,*,#4668,.T.);
#6104=ORIENTED_EDGE('',*,*,#4669,.T.);
#6105=ORIENTED_EDGE('',*,*,#4670,.T.);
#6106=ORIENTED_EDGE('',*,*,#4671,.T.);
#6107=ORIENTED_EDGE('',*,*,#4672,.T.);
#6108=ORIENTED_EDGE('',*,*,#4673,.T.);
#6109=ORIENTED_EDGE('',*,*,#4674,.T.);
#6110=ORIENTED_EDGE('',*,*,#4675,.T.);
#6111=ORIENTED_EDGE('',*,*,#4676,.T.);
#6112=ORIENTED_EDGE('',*,*,#4677,.T.);
#6113=ORIENTED_EDGE('',*,*,#4678,.T.);
#6114=ORIENTED_EDGE('',*,*,#4679,.T.);
#6115=ORIENTED_EDGE('',*,*,#4680,.T.);
#6116=ORIENTED_EDGE('',*,*,#4681,.T.);
#6117=ORIENTED_EDGE('',*,*,#4682,.T.);
#6118=ORIENTED_EDGE('',*,*,#4683,.T.);
#6119=ORIENTED_EDGE('',*,*,#4684,.T.);
#6120=ORIENTED_EDGE('',*,*,#4685,.T.);
#6121=ORIENTED_EDGE('',*,*,#4686,.T.);
#6122=ORIENTED_EDGE('',*,*,#4687,.T.);
#6123=ORIENTED_EDGE('',*,*,#4688,.T.);
#6124=ORIENTED_EDGE('',*,*,#4689,.T.);
#6125=ORIENTED_EDGE('',*,*,#4690,.T.);
#6126=ORIENTED_EDGE('',*,*,#4691,.T.);
#6127=ORIENTED_EDGE('',*,*,#4692,.T.);
#6128=ORIENTED_EDGE('',*,*,#4693,.T.);
#6129=ORIENTED_EDGE('',*,*,#4694,.T.);
#6130=ORIENTED_EDGE('',*,*,#4695,.T.);
#6131=ORIENTED_EDGE('',*,*,#4696,.T.);
#6132=ORIENTED_EDGE('',*,*,#4697,.T.);
#6133=ORIENTED_EDGE('',*,*,#4698,.T.);
#6134=ORIENTED_EDGE('',*,*,#4699,.T.);
#6135=ORIENTED_EDGE('',*,*,#4700,.T.);
#6136=ORIENTED_EDGE('',*,*,#4701,.T.);
#6137=ORIENTED_EDGE('',*,*,#4702,.T.);
#6138=ORIENTED_EDGE('',*,*,#4703,.T.);
#6139=ORIENTED_EDGE('',*,*,#4704,.T.);
#6140=ORIENTED_EDGE('',*,*,#4705,.T.);
#6141=ORIENTED_EDGE('',*,*,#4706,.T.);
#6142=ORIENTED_EDGE('',*,*,#4707,.T.);
#6143=ORIENTED_EDGE('',*,*,#4708,.T.);
#6144=ORIENTED_EDGE('',*,*,#4709,.T.);
#6145=ORIENTED_EDGE('',*,*,#4710,.T.);
#6146=ORIENTED_EDGE('',*,*,#4711,.T.);
#6147=ORIENTED_EDGE('',*,*,#4712,.T.);
#6148=ORIENTED_EDGE('',*,*,#4713,.T.);
#6149=ORIENTED_EDGE('',*,*,#4714,.T.);
#6150=ORIENTED_EDGE('',*,*,#4715,.T.);
#6151=ORIENTED_EDGE('',*,*,#4716,.T.);
#6152=ORIENTED_EDGE('',*,*,#4717,.T.);
#6153=ORIENTED_EDGE('',*,*,#4718,.T.);
#6154=ORIENTED_EDGE('',*,*,#4719,.T.);
#6155=ORIENTED_EDGE('',*,*,#4720,.T.);
#6156=ORIENTED_EDGE('',*,*,#4721,.T.);
#6157=ORIENTED_EDGE('',*,*,#4722,.T.);
#6158=ORIENTED_EDGE('',*,*,#4723,.T.);
#6159=ORIENTED_EDGE('',*,*,#4724,.T.);
#6160=ORIENTED_EDGE('',*,*,#4725,.T.);
#6161=ORIENTED_EDGE('',*,*,#4726,.T.);
#6162=ORIENTED_EDGE('',*,*,#4727,.T.);
#6163=ORIENTED_EDGE('',*,*,#4728,.T.);
#6164=ORIENTED_EDGE('',*,*,#4621,.F.);
#6165=ORIENTED_EDGE('',*,*,#4729,.T.);
#6166=ORIENTED_EDGE('',*,*,#4730,.T.);
#6167=ORIENTED_EDGE('',*,*,#4729,.F.);
#6168=ORIENTED_EDGE('',*,*,#4731,.T.);
#6169=ORIENTED_EDGE('',*,*,#4732,.T.);
#6170=ORIENTED_EDGE('',*,*,#4733,.T.);
#6171=ORIENTED_EDGE('',*,*,#4734,.T.);
#6172=ORIENTED_EDGE('',*,*,#4617,.T.);
#6173=ORIENTED_EDGE('',*,*,#4632,.T.);
#6174=ORIENTED_EDGE('',*,*,#4735,.T.);
#6175=ORIENTED_EDGE('',*,*,#4732,.F.);
#6176=ORIENTED_EDGE('',*,*,#4731,.F.);
#6177=ORIENTED_EDGE('',*,*,#4736,.T.);
#6178=ORIENTED_EDGE('',*,*,#4737,.T.);
#6179=ORIENTED_EDGE('',*,*,#4736,.F.);
#6180=ORIENTED_EDGE('',*,*,#4738,.T.);
#6181=ORIENTED_EDGE('',*,*,#4647,.T.);
#6182=ORIENTED_EDGE('',*,*,#4739,.T.);
#6183=ORIENTED_EDGE('',*,*,#4740,.T.);
#6184=ORIENTED_EDGE('',*,*,#4741,.T.);
#6185=ORIENTED_EDGE('',*,*,#4574,.T.);
#6186=ORIENTED_EDGE('',*,*,#4741,.F.);
#6187=ORIENTED_EDGE('',*,*,#4742,.T.);
#6188=ORIENTED_EDGE('',*,*,#4743,.T.);
#6189=ORIENTED_EDGE('',*,*,#4575,.F.);
#6190=ORIENTED_EDGE('',*,*,#4740,.F.);
#6191=ORIENTED_EDGE('',*,*,#4744,.T.);
#6192=ORIENTED_EDGE('',*,*,#4745,.T.);
#6193=ORIENTED_EDGE('',*,*,#4742,.F.);
#6194=ORIENTED_EDGE('',*,*,#4612,.F.);
#6195=ORIENTED_EDGE('',*,*,#4615,.T.);
#6196=ORIENTED_EDGE('',*,*,#4583,.T.);
#6197=ORIENTED_EDGE('',*,*,#4588,.T.);
#6198=ORIENTED_EDGE('',*,*,#4633,.T.);
#6199=ORIENTED_EDGE('',*,*,#4734,.F.);
#6200=ORIENTED_EDGE('',*,*,#4746,.T.);
#6201=ORIENTED_EDGE('',*,*,#4563,.T.);
#6202=ORIENTED_EDGE('',*,*,#4618,.F.);
#6203=ORIENTED_EDGE('',*,*,#4627,.F.);
#6204=ORIENTED_EDGE('',*,*,#4747,.T.);
#6205=ORIENTED_EDGE('',*,*,#4748,.T.);
#6206=ORIENTED_EDGE('',*,*,#4746,.F.);
#6207=ORIENTED_EDGE('',*,*,#4733,.F.);
#6208=ORIENTED_EDGE('',*,*,#4735,.F.);
#6209=ORIENTED_EDGE('',*,*,#4631,.T.);
#6210=ORIENTED_EDGE('',*,*,#4623,.F.);
#6211=ORIENTED_EDGE('',*,*,#4626,.F.);
#6212=ORIENTED_EDGE('',*,*,#4629,.T.);
#6213=ORIENTED_EDGE('',*,*,#4749,.T.);
#6214=ORIENTED_EDGE('',*,*,#4747,.F.);
#6215=ORIENTED_EDGE('',*,*,#4544,.F.);
#6216=ORIENTED_EDGE('',*,*,#4564,.F.);
#6217=ORIENTED_EDGE('',*,*,#4748,.F.);
#6218=ORIENTED_EDGE('',*,*,#4750,.F.);
#6219=ORIENTED_EDGE('',*,*,#4542,.F.);
#6220=ORIENTED_EDGE('',*,*,#4750,.T.);
#6221=ORIENTED_EDGE('',*,*,#4749,.F.);
#6222=ORIENTED_EDGE('',*,*,#4751,.T.);
#6223=ORIENTED_EDGE('',*,*,#4538,.F.);
#6224=ORIENTED_EDGE('',*,*,#4751,.F.);
#6225=ORIENTED_EDGE('',*,*,#4628,.F.);
#6226=ORIENTED_EDGE('',*,*,#4752,.T.);
#6227=ORIENTED_EDGE('',*,*,#4559,.F.);
#6228=ORIENTED_EDGE('',*,*,#4752,.F.);
#6229=ORIENTED_EDGE('',*,*,#4599,.F.);
#6230=ORIENTED_EDGE('',*,*,#4569,.T.);
#6231=ORIENTED_EDGE('',*,*,#4604,.F.);
#6232=ORIENTED_EDGE('',*,*,#4753,.T.);
#6233=ORIENTED_EDGE('',*,*,#4754,.T.);
#6234=ORIENTED_EDGE('',*,*,#4571,.F.);
#6235=ORIENTED_EDGE('',*,*,#4603,.F.);
#6236=ORIENTED_EDGE('',*,*,#4755,.T.);
#6237=ORIENTED_EDGE('',*,*,#4756,.T.);
#6238=ORIENTED_EDGE('',*,*,#4753,.F.);
#6239=ORIENTED_EDGE('',*,*,#4590,.F.);
#6240=ORIENTED_EDGE('',*,*,#4757,.F.);
#6241=ORIENTED_EDGE('',*,*,#4758,.F.);
#6242=ORIENTED_EDGE('',*,*,#4759,.F.);
#6243=ORIENTED_EDGE('',*,*,#4760,.F.);
#6244=ORIENTED_EDGE('',*,*,#4761,.F.);
#6245=ORIENTED_EDGE('',*,*,#4762,.F.);
#6246=ORIENTED_EDGE('',*,*,#4585,.F.);
#6247=ORIENTED_EDGE('',*,*,#4602,.F.);
#6248=ORIENTED_EDGE('',*,*,#4654,.F.);
#6249=ORIENTED_EDGE('',*,*,#4763,.T.);
#6250=ORIENTED_EDGE('',*,*,#4764,.T.);
#6251=ORIENTED_EDGE('',*,*,#4755,.F.);
#6252=ORIENTED_EDGE('',*,*,#4653,.F.);
#6253=ORIENTED_EDGE('',*,*,#4765,.T.);
#6254=ORIENTED_EDGE('',*,*,#4766,.T.);
#6255=ORIENTED_EDGE('',*,*,#4763,.F.);
#6256=ORIENTED_EDGE('',*,*,#4652,.F.);
#6257=ORIENTED_EDGE('',*,*,#4767,.T.);
#6258=ORIENTED_EDGE('',*,*,#4768,.T.);
#6259=ORIENTED_EDGE('',*,*,#4765,.F.);
#6260=ORIENTED_EDGE('',*,*,#4651,.F.);
#6261=ORIENTED_EDGE('',*,*,#4769,.T.);
#6262=ORIENTED_EDGE('',*,*,#4770,.T.);
#6263=ORIENTED_EDGE('',*,*,#4767,.F.);
#6264=ORIENTED_EDGE('',*,*,#4650,.F.);
#6265=ORIENTED_EDGE('',*,*,#4771,.T.);
#6266=ORIENTED_EDGE('',*,*,#4772,.T.);
#6267=ORIENTED_EDGE('',*,*,#4769,.F.);
#6268=ORIENTED_EDGE('',*,*,#4649,.F.);
#6269=ORIENTED_EDGE('',*,*,#4773,.T.);
#6270=ORIENTED_EDGE('',*,*,#4774,.T.);
#6271=ORIENTED_EDGE('',*,*,#4771,.F.);
#6272=ORIENTED_EDGE('',*,*,#4738,.F.);
#6273=ORIENTED_EDGE('',*,*,#4573,.F.);
#6274=ORIENTED_EDGE('',*,*,#4775,.T.);
#6275=ORIENTED_EDGE('',*,*,#4773,.F.);
#6276=ORIENTED_EDGE('',*,*,#4648,.F.);
#6277=ORIENTED_EDGE('',*,*,#4572,.F.);
#6278=ORIENTED_EDGE('',*,*,#4754,.F.);
#6279=ORIENTED_EDGE('',*,*,#4756,.F.);
#6280=ORIENTED_EDGE('',*,*,#4764,.F.);
#6281=ORIENTED_EDGE('',*,*,#4766,.F.);
#6282=ORIENTED_EDGE('',*,*,#4768,.F.);
#6283=ORIENTED_EDGE('',*,*,#4770,.F.);
#6284=ORIENTED_EDGE('',*,*,#4772,.F.);
#6285=ORIENTED_EDGE('',*,*,#4774,.F.);
#6286=ORIENTED_EDGE('',*,*,#4775,.F.);
#6287=ORIENTED_EDGE('',*,*,#4739,.F.);
#6288=ORIENTED_EDGE('',*,*,#4646,.F.);
#6289=ORIENTED_EDGE('',*,*,#4776,.T.);
#6290=ORIENTED_EDGE('',*,*,#4777,.T.);
#6291=ORIENTED_EDGE('',*,*,#4744,.F.);
#6292=ORIENTED_EDGE('',*,*,#4645,.F.);
#6293=ORIENTED_EDGE('',*,*,#4778,.T.);
#6294=ORIENTED_EDGE('',*,*,#4779,.T.);
#6295=ORIENTED_EDGE('',*,*,#4776,.F.);
#6296=ORIENTED_EDGE('',*,*,#4644,.F.);
#6297=ORIENTED_EDGE('',*,*,#4780,.T.);
#6298=ORIENTED_EDGE('',*,*,#4781,.T.);
#6299=ORIENTED_EDGE('',*,*,#4778,.F.);
#6300=ORIENTED_EDGE('',*,*,#4643,.F.);
#6301=ORIENTED_EDGE('',*,*,#4782,.T.);
#6302=ORIENTED_EDGE('',*,*,#4783,.T.);
#6303=ORIENTED_EDGE('',*,*,#4780,.F.);
#6304=ORIENTED_EDGE('',*,*,#4642,.F.);
#6305=ORIENTED_EDGE('',*,*,#4784,.T.);
#6306=ORIENTED_EDGE('',*,*,#4785,.T.);
#6307=ORIENTED_EDGE('',*,*,#4782,.F.);
#6308=ORIENTED_EDGE('',*,*,#4641,.F.);
#6309=ORIENTED_EDGE('',*,*,#4786,.T.);
#6310=ORIENTED_EDGE('',*,*,#4787,.T.);
#6311=ORIENTED_EDGE('',*,*,#4784,.F.);
#6312=ORIENTED_EDGE('',*,*,#4577,.F.);
#6313=ORIENTED_EDGE('',*,*,#4788,.T.);
#6314=ORIENTED_EDGE('',*,*,#4786,.F.);
#6315=ORIENTED_EDGE('',*,*,#4640,.F.);
#6316=ORIENTED_EDGE('',*,*,#4576,.F.);
#6317=ORIENTED_EDGE('',*,*,#4743,.F.);
#6318=ORIENTED_EDGE('',*,*,#4745,.F.);
#6319=ORIENTED_EDGE('',*,*,#4777,.F.);
#6320=ORIENTED_EDGE('',*,*,#4779,.F.);
#6321=ORIENTED_EDGE('',*,*,#4781,.F.);
#6322=ORIENTED_EDGE('',*,*,#4783,.F.);
#6323=ORIENTED_EDGE('',*,*,#4785,.F.);
#6324=ORIENTED_EDGE('',*,*,#4787,.F.);
#6325=ORIENTED_EDGE('',*,*,#4788,.F.);
#6326=ORIENTED_EDGE('',*,*,#4557,.F.);
#6327=ORIENTED_EDGE('',*,*,#4580,.T.);
#6328=ORIENTED_EDGE('',*,*,#4579,.F.);
#6329=ORIENTED_EDGE('',*,*,#4639,.F.);
#6330=ORIENTED_EDGE('',*,*,#4789,.T.);
#6331=ORIENTED_EDGE('',*,*,#4757,.T.);
#6332=ORIENTED_EDGE('',*,*,#4589,.F.);
#6333=ORIENTED_EDGE('',*,*,#4638,.F.);
#6334=ORIENTED_EDGE('',*,*,#4790,.T.);
#6335=ORIENTED_EDGE('',*,*,#4758,.T.);
#6336=ORIENTED_EDGE('',*,*,#4789,.F.);
#6337=ORIENTED_EDGE('',*,*,#4637,.F.);
#6338=ORIENTED_EDGE('',*,*,#4791,.T.);
#6339=ORIENTED_EDGE('',*,*,#4759,.T.);
#6340=ORIENTED_EDGE('',*,*,#4790,.F.);
#6341=ORIENTED_EDGE('',*,*,#4636,.F.);
#6342=ORIENTED_EDGE('',*,*,#4792,.T.);
#6343=ORIENTED_EDGE('',*,*,#4760,.T.);
#6344=ORIENTED_EDGE('',*,*,#4791,.F.);
#6345=ORIENTED_EDGE('',*,*,#4635,.F.);
#6346=ORIENTED_EDGE('',*,*,#4793,.T.);
#6347=ORIENTED_EDGE('',*,*,#4761,.T.);
#6348=ORIENTED_EDGE('',*,*,#4792,.F.);
#6349=ORIENTED_EDGE('',*,*,#4634,.F.);
#6350=ORIENTED_EDGE('',*,*,#4586,.T.);
#6351=ORIENTED_EDGE('',*,*,#4762,.T.);
#6352=ORIENTED_EDGE('',*,*,#4793,.F.);
#6353=ORIENTED_EDGE('',*,*,#4655,.F.);
#6354=ORIENTED_EDGE('',*,*,#4794,.T.);
#6355=ORIENTED_EDGE('',*,*,#4795,.T.);
#6356=ORIENTED_EDGE('',*,*,#4796,.F.);
#6357=ORIENTED_EDGE('',*,*,#4664,.F.);
#6358=ORIENTED_EDGE('',*,*,#4797,.T.);
#6359=ORIENTED_EDGE('',*,*,#4798,.T.);
#6360=ORIENTED_EDGE('',*,*,#4794,.F.);
#6361=ORIENTED_EDGE('',*,*,#4663,.F.);
#6362=ORIENTED_EDGE('',*,*,#4799,.T.);
#6363=ORIENTED_EDGE('',*,*,#4800,.T.);
#6364=ORIENTED_EDGE('',*,*,#4797,.F.);
#6365=ORIENTED_EDGE('',*,*,#4662,.F.);
#6366=ORIENTED_EDGE('',*,*,#4801,.T.);
#6367=ORIENTED_EDGE('',*,*,#4802,.T.);
#6368=ORIENTED_EDGE('',*,*,#4799,.F.);
#6369=ORIENTED_EDGE('',*,*,#4661,.F.);
#6370=ORIENTED_EDGE('',*,*,#4803,.T.);
#6371=ORIENTED_EDGE('',*,*,#4804,.T.);
#6372=ORIENTED_EDGE('',*,*,#4801,.F.);
#6373=ORIENTED_EDGE('',*,*,#4660,.F.);
#6374=ORIENTED_EDGE('',*,*,#4805,.T.);
#6375=ORIENTED_EDGE('',*,*,#4806,.T.);
#6376=ORIENTED_EDGE('',*,*,#4803,.F.);
#6377=ORIENTED_EDGE('',*,*,#4659,.F.);
#6378=ORIENTED_EDGE('',*,*,#4807,.T.);
#6379=ORIENTED_EDGE('',*,*,#4808,.T.);
#6380=ORIENTED_EDGE('',*,*,#4805,.F.);
#6381=ORIENTED_EDGE('',*,*,#4658,.F.);
#6382=ORIENTED_EDGE('',*,*,#4809,.T.);
#6383=ORIENTED_EDGE('',*,*,#4810,.T.);
#6384=ORIENTED_EDGE('',*,*,#4807,.F.);
#6385=ORIENTED_EDGE('',*,*,#4657,.F.);
#6386=ORIENTED_EDGE('',*,*,#4811,.T.);
#6387=ORIENTED_EDGE('',*,*,#4812,.T.);
#6388=ORIENTED_EDGE('',*,*,#4809,.F.);
#6389=ORIENTED_EDGE('',*,*,#4656,.F.);
#6390=ORIENTED_EDGE('',*,*,#4796,.T.);
#6391=ORIENTED_EDGE('',*,*,#4813,.T.);
#6392=ORIENTED_EDGE('',*,*,#4811,.F.);
#6393=ORIENTED_EDGE('',*,*,#4813,.F.);
#6394=ORIENTED_EDGE('',*,*,#4795,.F.);
#6395=ORIENTED_EDGE('',*,*,#4798,.F.);
#6396=ORIENTED_EDGE('',*,*,#4800,.F.);
#6397=ORIENTED_EDGE('',*,*,#4802,.F.);
#6398=ORIENTED_EDGE('',*,*,#4804,.F.);
#6399=ORIENTED_EDGE('',*,*,#4806,.F.);
#6400=ORIENTED_EDGE('',*,*,#4808,.F.);
#6401=ORIENTED_EDGE('',*,*,#4810,.F.);
#6402=ORIENTED_EDGE('',*,*,#4812,.F.);
#6403=ORIENTED_EDGE('',*,*,#4665,.F.);
#6404=ORIENTED_EDGE('',*,*,#4814,.T.);
#6405=ORIENTED_EDGE('',*,*,#4815,.T.);
#6406=ORIENTED_EDGE('',*,*,#4816,.F.);
#6407=ORIENTED_EDGE('',*,*,#4674,.F.);
#6408=ORIENTED_EDGE('',*,*,#4817,.T.);
#6409=ORIENTED_EDGE('',*,*,#4818,.T.);
#6410=ORIENTED_EDGE('',*,*,#4814,.F.);
#6411=ORIENTED_EDGE('',*,*,#4673,.F.);
#6412=ORIENTED_EDGE('',*,*,#4819,.T.);
#6413=ORIENTED_EDGE('',*,*,#4820,.T.);
#6414=ORIENTED_EDGE('',*,*,#4817,.F.);
#6415=ORIENTED_EDGE('',*,*,#4672,.F.);
#6416=ORIENTED_EDGE('',*,*,#4821,.T.);
#6417=ORIENTED_EDGE('',*,*,#4822,.T.);
#6418=ORIENTED_EDGE('',*,*,#4819,.F.);
#6419=ORIENTED_EDGE('',*,*,#4671,.F.);
#6420=ORIENTED_EDGE('',*,*,#4823,.T.);
#6421=ORIENTED_EDGE('',*,*,#4824,.T.);
#6422=ORIENTED_EDGE('',*,*,#4821,.F.);
#6423=ORIENTED_EDGE('',*,*,#4670,.F.);
#6424=ORIENTED_EDGE('',*,*,#4825,.T.);
#6425=ORIENTED_EDGE('',*,*,#4826,.T.);
#6426=ORIENTED_EDGE('',*,*,#4823,.F.);
#6427=ORIENTED_EDGE('',*,*,#4669,.F.);
#6428=ORIENTED_EDGE('',*,*,#4827,.T.);
#6429=ORIENTED_EDGE('',*,*,#4828,.T.);
#6430=ORIENTED_EDGE('',*,*,#4825,.F.);
#6431=ORIENTED_EDGE('',*,*,#4668,.F.);
#6432=ORIENTED_EDGE('',*,*,#4829,.T.);
#6433=ORIENTED_EDGE('',*,*,#4830,.T.);
#6434=ORIENTED_EDGE('',*,*,#4827,.F.);
#6435=ORIENTED_EDGE('',*,*,#4667,.F.);
#6436=ORIENTED_EDGE('',*,*,#4831,.T.);
#6437=ORIENTED_EDGE('',*,*,#4832,.T.);
#6438=ORIENTED_EDGE('',*,*,#4829,.F.);
#6439=ORIENTED_EDGE('',*,*,#4666,.F.);
#6440=ORIENTED_EDGE('',*,*,#4816,.T.);
#6441=ORIENTED_EDGE('',*,*,#4833,.T.);
#6442=ORIENTED_EDGE('',*,*,#4831,.F.);
#6443=ORIENTED_EDGE('',*,*,#4833,.F.);
#6444=ORIENTED_EDGE('',*,*,#4815,.F.);
#6445=ORIENTED_EDGE('',*,*,#4818,.F.);
#6446=ORIENTED_EDGE('',*,*,#4820,.F.);
#6447=ORIENTED_EDGE('',*,*,#4822,.F.);
#6448=ORIENTED_EDGE('',*,*,#4824,.F.);
#6449=ORIENTED_EDGE('',*,*,#4826,.F.);
#6450=ORIENTED_EDGE('',*,*,#4828,.F.);
#6451=ORIENTED_EDGE('',*,*,#4830,.F.);
#6452=ORIENTED_EDGE('',*,*,#4832,.F.);
#6453=ORIENTED_EDGE('',*,*,#4675,.F.);
#6454=ORIENTED_EDGE('',*,*,#4834,.T.);
#6455=ORIENTED_EDGE('',*,*,#4835,.T.);
#6456=ORIENTED_EDGE('',*,*,#4836,.F.);
#6457=ORIENTED_EDGE('',*,*,#4685,.F.);
#6458=ORIENTED_EDGE('',*,*,#4837,.T.);
#6459=ORIENTED_EDGE('',*,*,#4838,.T.);
#6460=ORIENTED_EDGE('',*,*,#4834,.F.);
#6461=ORIENTED_EDGE('',*,*,#4684,.F.);
#6462=ORIENTED_EDGE('',*,*,#4839,.T.);
#6463=ORIENTED_EDGE('',*,*,#4840,.T.);
#6464=ORIENTED_EDGE('',*,*,#4837,.F.);
#6465=ORIENTED_EDGE('',*,*,#4683,.F.);
#6466=ORIENTED_EDGE('',*,*,#4841,.T.);
#6467=ORIENTED_EDGE('',*,*,#4842,.T.);
#6468=ORIENTED_EDGE('',*,*,#4839,.F.);
#6469=ORIENTED_EDGE('',*,*,#4682,.F.);
#6470=ORIENTED_EDGE('',*,*,#4843,.T.);
#6471=ORIENTED_EDGE('',*,*,#4844,.T.);
#6472=ORIENTED_EDGE('',*,*,#4841,.F.);
#6473=ORIENTED_EDGE('',*,*,#4681,.F.);
#6474=ORIENTED_EDGE('',*,*,#4845,.T.);
#6475=ORIENTED_EDGE('',*,*,#4846,.T.);
#6476=ORIENTED_EDGE('',*,*,#4843,.F.);
#6477=ORIENTED_EDGE('',*,*,#4680,.F.);
#6478=ORIENTED_EDGE('',*,*,#4847,.T.);
#6479=ORIENTED_EDGE('',*,*,#4848,.T.);
#6480=ORIENTED_EDGE('',*,*,#4845,.F.);
#6481=ORIENTED_EDGE('',*,*,#4679,.F.);
#6482=ORIENTED_EDGE('',*,*,#4849,.T.);
#6483=ORIENTED_EDGE('',*,*,#4850,.T.);
#6484=ORIENTED_EDGE('',*,*,#4847,.F.);
#6485=ORIENTED_EDGE('',*,*,#4678,.F.);
#6486=ORIENTED_EDGE('',*,*,#4851,.T.);
#6487=ORIENTED_EDGE('',*,*,#4852,.T.);
#6488=ORIENTED_EDGE('',*,*,#4849,.F.);
#6489=ORIENTED_EDGE('',*,*,#4677,.F.);
#6490=ORIENTED_EDGE('',*,*,#4853,.T.);
#6491=ORIENTED_EDGE('',*,*,#4854,.T.);
#6492=ORIENTED_EDGE('',*,*,#4851,.F.);
#6493=ORIENTED_EDGE('',*,*,#4676,.F.);
#6494=ORIENTED_EDGE('',*,*,#4836,.T.);
#6495=ORIENTED_EDGE('',*,*,#4855,.T.);
#6496=ORIENTED_EDGE('',*,*,#4853,.F.);
#6497=ORIENTED_EDGE('',*,*,#4855,.F.);
#6498=ORIENTED_EDGE('',*,*,#4835,.F.);
#6499=ORIENTED_EDGE('',*,*,#4838,.F.);
#6500=ORIENTED_EDGE('',*,*,#4840,.F.);
#6501=ORIENTED_EDGE('',*,*,#4842,.F.);
#6502=ORIENTED_EDGE('',*,*,#4844,.F.);
#6503=ORIENTED_EDGE('',*,*,#4846,.F.);
#6504=ORIENTED_EDGE('',*,*,#4848,.F.);
#6505=ORIENTED_EDGE('',*,*,#4850,.F.);
#6506=ORIENTED_EDGE('',*,*,#4852,.F.);
#6507=ORIENTED_EDGE('',*,*,#4854,.F.);
#6508=ORIENTED_EDGE('',*,*,#4719,.F.);
#6509=ORIENTED_EDGE('',*,*,#4856,.T.);
#6510=ORIENTED_EDGE('',*,*,#4857,.T.);
#6511=ORIENTED_EDGE('',*,*,#4858,.F.);
#6512=ORIENTED_EDGE('',*,*,#4728,.F.);
#6513=ORIENTED_EDGE('',*,*,#4859,.T.);
#6514=ORIENTED_EDGE('',*,*,#4860,.T.);
#6515=ORIENTED_EDGE('',*,*,#4856,.F.);
#6516=ORIENTED_EDGE('',*,*,#4727,.F.);
#6517=ORIENTED_EDGE('',*,*,#4861,.T.);
#6518=ORIENTED_EDGE('',*,*,#4862,.T.);
#6519=ORIENTED_EDGE('',*,*,#4859,.F.);
#6520=ORIENTED_EDGE('',*,*,#4726,.F.);
#6521=ORIENTED_EDGE('',*,*,#4863,.T.);
#6522=ORIENTED_EDGE('',*,*,#4864,.T.);
#6523=ORIENTED_EDGE('',*,*,#4861,.F.);
#6524=ORIENTED_EDGE('',*,*,#4725,.F.);
#6525=ORIENTED_EDGE('',*,*,#4865,.T.);
#6526=ORIENTED_EDGE('',*,*,#4866,.T.);
#6527=ORIENTED_EDGE('',*,*,#4863,.F.);
#6528=ORIENTED_EDGE('',*,*,#4724,.F.);
#6529=ORIENTED_EDGE('',*,*,#4867,.T.);
#6530=ORIENTED_EDGE('',*,*,#4868,.T.);
#6531=ORIENTED_EDGE('',*,*,#4865,.F.);
#6532=ORIENTED_EDGE('',*,*,#4723,.F.);
#6533=ORIENTED_EDGE('',*,*,#4869,.T.);
#6534=ORIENTED_EDGE('',*,*,#4870,.T.);
#6535=ORIENTED_EDGE('',*,*,#4867,.F.);
#6536=ORIENTED_EDGE('',*,*,#4722,.F.);
#6537=ORIENTED_EDGE('',*,*,#4871,.T.);
#6538=ORIENTED_EDGE('',*,*,#4872,.T.);
#6539=ORIENTED_EDGE('',*,*,#4869,.F.);
#6540=ORIENTED_EDGE('',*,*,#4721,.F.);
#6541=ORIENTED_EDGE('',*,*,#4873,.T.);
#6542=ORIENTED_EDGE('',*,*,#4874,.T.);
#6543=ORIENTED_EDGE('',*,*,#4871,.F.);
#6544=ORIENTED_EDGE('',*,*,#4720,.F.);
#6545=ORIENTED_EDGE('',*,*,#4858,.T.);
#6546=ORIENTED_EDGE('',*,*,#4875,.T.);
#6547=ORIENTED_EDGE('',*,*,#4873,.F.);
#6548=ORIENTED_EDGE('',*,*,#4875,.F.);
#6549=ORIENTED_EDGE('',*,*,#4857,.F.);
#6550=ORIENTED_EDGE('',*,*,#4860,.F.);
#6551=ORIENTED_EDGE('',*,*,#4862,.F.);
#6552=ORIENTED_EDGE('',*,*,#4864,.F.);
#6553=ORIENTED_EDGE('',*,*,#4866,.F.);
#6554=ORIENTED_EDGE('',*,*,#4868,.F.);
#6555=ORIENTED_EDGE('',*,*,#4870,.F.);
#6556=ORIENTED_EDGE('',*,*,#4872,.F.);
#6557=ORIENTED_EDGE('',*,*,#4874,.F.);
#6558=ORIENTED_EDGE('',*,*,#4708,.F.);
#6559=ORIENTED_EDGE('',*,*,#4876,.T.);
#6560=ORIENTED_EDGE('',*,*,#4877,.T.);
#6561=ORIENTED_EDGE('',*,*,#4878,.F.);
#6562=ORIENTED_EDGE('',*,*,#4718,.F.);
#6563=ORIENTED_EDGE('',*,*,#4879,.T.);
#6564=ORIENTED_EDGE('',*,*,#4880,.T.);
#6565=ORIENTED_EDGE('',*,*,#4876,.F.);
#6566=ORIENTED_EDGE('',*,*,#4717,.F.);
#6567=ORIENTED_EDGE('',*,*,#4881,.T.);
#6568=ORIENTED_EDGE('',*,*,#4882,.T.);
#6569=ORIENTED_EDGE('',*,*,#4879,.F.);
#6570=ORIENTED_EDGE('',*,*,#4716,.F.);
#6571=ORIENTED_EDGE('',*,*,#4883,.T.);
#6572=ORIENTED_EDGE('',*,*,#4884,.T.);
#6573=ORIENTED_EDGE('',*,*,#4881,.F.);
#6574=ORIENTED_EDGE('',*,*,#4715,.F.);
#6575=ORIENTED_EDGE('',*,*,#4885,.T.);
#6576=ORIENTED_EDGE('',*,*,#4886,.T.);
#6577=ORIENTED_EDGE('',*,*,#4883,.F.);
#6578=ORIENTED_EDGE('',*,*,#4714,.F.);
#6579=ORIENTED_EDGE('',*,*,#4887,.T.);
#6580=ORIENTED_EDGE('',*,*,#4888,.T.);
#6581=ORIENTED_EDGE('',*,*,#4885,.F.);
#6582=ORIENTED_EDGE('',*,*,#4713,.F.);
#6583=ORIENTED_EDGE('',*,*,#4889,.T.);
#6584=ORIENTED_EDGE('',*,*,#4890,.T.);
#6585=ORIENTED_EDGE('',*,*,#4887,.F.);
#6586=ORIENTED_EDGE('',*,*,#4712,.F.);
#6587=ORIENTED_EDGE('',*,*,#4891,.T.);
#6588=ORIENTED_EDGE('',*,*,#4892,.T.);
#6589=ORIENTED_EDGE('',*,*,#4889,.F.);
#6590=ORIENTED_EDGE('',*,*,#4711,.F.);
#6591=ORIENTED_EDGE('',*,*,#4893,.T.);
#6592=ORIENTED_EDGE('',*,*,#4894,.T.);
#6593=ORIENTED_EDGE('',*,*,#4891,.F.);
#6594=ORIENTED_EDGE('',*,*,#4710,.F.);
#6595=ORIENTED_EDGE('',*,*,#4895,.T.);
#6596=ORIENTED_EDGE('',*,*,#4896,.T.);
#6597=ORIENTED_EDGE('',*,*,#4893,.F.);
#6598=ORIENTED_EDGE('',*,*,#4709,.F.);
#6599=ORIENTED_EDGE('',*,*,#4878,.T.);
#6600=ORIENTED_EDGE('',*,*,#4897,.T.);
#6601=ORIENTED_EDGE('',*,*,#4895,.F.);
#6602=ORIENTED_EDGE('',*,*,#4897,.F.);
#6603=ORIENTED_EDGE('',*,*,#4877,.F.);
#6604=ORIENTED_EDGE('',*,*,#4880,.F.);
#6605=ORIENTED_EDGE('',*,*,#4882,.F.);
#6606=ORIENTED_EDGE('',*,*,#4884,.F.);
#6607=ORIENTED_EDGE('',*,*,#4886,.F.);
#6608=ORIENTED_EDGE('',*,*,#4888,.F.);
#6609=ORIENTED_EDGE('',*,*,#4890,.F.);
#6610=ORIENTED_EDGE('',*,*,#4892,.F.);
#6611=ORIENTED_EDGE('',*,*,#4894,.F.);
#6612=ORIENTED_EDGE('',*,*,#4896,.F.);
#6613=ORIENTED_EDGE('',*,*,#4686,.F.);
#6614=ORIENTED_EDGE('',*,*,#4898,.T.);
#6615=ORIENTED_EDGE('',*,*,#4899,.T.);
#6616=ORIENTED_EDGE('',*,*,#4900,.F.);
#6617=ORIENTED_EDGE('',*,*,#4695,.F.);
#6618=ORIENTED_EDGE('',*,*,#4901,.T.);
#6619=ORIENTED_EDGE('',*,*,#4902,.T.);
#6620=ORIENTED_EDGE('',*,*,#4898,.F.);
#6621=ORIENTED_EDGE('',*,*,#4694,.F.);
#6622=ORIENTED_EDGE('',*,*,#4903,.T.);
#6623=ORIENTED_EDGE('',*,*,#4904,.T.);
#6624=ORIENTED_EDGE('',*,*,#4901,.F.);
#6625=ORIENTED_EDGE('',*,*,#4693,.F.);
#6626=ORIENTED_EDGE('',*,*,#4905,.T.);
#6627=ORIENTED_EDGE('',*,*,#4906,.T.);
#6628=ORIENTED_EDGE('',*,*,#4903,.F.);
#6629=ORIENTED_EDGE('',*,*,#4692,.F.);
#6630=ORIENTED_EDGE('',*,*,#4907,.T.);
#6631=ORIENTED_EDGE('',*,*,#4908,.T.);
#6632=ORIENTED_EDGE('',*,*,#4905,.F.);
#6633=ORIENTED_EDGE('',*,*,#4691,.F.);
#6634=ORIENTED_EDGE('',*,*,#4909,.T.);
#6635=ORIENTED_EDGE('',*,*,#4910,.T.);
#6636=ORIENTED_EDGE('',*,*,#4907,.F.);
#6637=ORIENTED_EDGE('',*,*,#4690,.F.);
#6638=ORIENTED_EDGE('',*,*,#4911,.T.);
#6639=ORIENTED_EDGE('',*,*,#4912,.T.);
#6640=ORIENTED_EDGE('',*,*,#4909,.F.);
#6641=ORIENTED_EDGE('',*,*,#4689,.F.);
#6642=ORIENTED_EDGE('',*,*,#4913,.T.);
#6643=ORIENTED_EDGE('',*,*,#4914,.T.);
#6644=ORIENTED_EDGE('',*,*,#4911,.F.);
#6645=ORIENTED_EDGE('',*,*,#4688,.F.);
#6646=ORIENTED_EDGE('',*,*,#4915,.T.);
#6647=ORIENTED_EDGE('',*,*,#4916,.T.);
#6648=ORIENTED_EDGE('',*,*,#4913,.F.);
#6649=ORIENTED_EDGE('',*,*,#4687,.F.);
#6650=ORIENTED_EDGE('',*,*,#4900,.T.);
#6651=ORIENTED_EDGE('',*,*,#4917,.T.);
#6652=ORIENTED_EDGE('',*,*,#4915,.F.);
#6653=ORIENTED_EDGE('',*,*,#4917,.F.);
#6654=ORIENTED_EDGE('',*,*,#4899,.F.);
#6655=ORIENTED_EDGE('',*,*,#4902,.F.);
#6656=ORIENTED_EDGE('',*,*,#4904,.F.);
#6657=ORIENTED_EDGE('',*,*,#4906,.F.);
#6658=ORIENTED_EDGE('',*,*,#4908,.F.);
#6659=ORIENTED_EDGE('',*,*,#4910,.F.);
#6660=ORIENTED_EDGE('',*,*,#4912,.F.);
#6661=ORIENTED_EDGE('',*,*,#4914,.F.);
#6662=ORIENTED_EDGE('',*,*,#4916,.F.);
#6663=ORIENTED_EDGE('',*,*,#4696,.F.);
#6664=ORIENTED_EDGE('',*,*,#4918,.T.);
#6665=ORIENTED_EDGE('',*,*,#4919,.T.);
#6666=ORIENTED_EDGE('',*,*,#4920,.F.);
#6667=ORIENTED_EDGE('',*,*,#4706,.F.);
#6668=ORIENTED_EDGE('',*,*,#4921,.T.);
#6669=ORIENTED_EDGE('',*,*,#4922,.T.);
#6670=ORIENTED_EDGE('',*,*,#4918,.F.);
#6671=ORIENTED_EDGE('',*,*,#4705,.F.);
#6672=ORIENTED_EDGE('',*,*,#4923,.T.);
#6673=ORIENTED_EDGE('',*,*,#4924,.T.);
#6674=ORIENTED_EDGE('',*,*,#4921,.F.);
#6675=ORIENTED_EDGE('',*,*,#4704,.F.);
#6676=ORIENTED_EDGE('',*,*,#4925,.T.);
#6677=ORIENTED_EDGE('',*,*,#4926,.T.);
#6678=ORIENTED_EDGE('',*,*,#4923,.F.);
#6679=ORIENTED_EDGE('',*,*,#4703,.F.);
#6680=ORIENTED_EDGE('',*,*,#4927,.T.);
#6681=ORIENTED_EDGE('',*,*,#4928,.T.);
#6682=ORIENTED_EDGE('',*,*,#4925,.F.);
#6683=ORIENTED_EDGE('',*,*,#4702,.F.);
#6684=ORIENTED_EDGE('',*,*,#4929,.T.);
#6685=ORIENTED_EDGE('',*,*,#4930,.T.);
#6686=ORIENTED_EDGE('',*,*,#4927,.F.);
#6687=ORIENTED_EDGE('',*,*,#4701,.F.);
#6688=ORIENTED_EDGE('',*,*,#4931,.T.);
#6689=ORIENTED_EDGE('',*,*,#4932,.T.);
#6690=ORIENTED_EDGE('',*,*,#4929,.F.);
#6691=ORIENTED_EDGE('',*,*,#4700,.F.);
#6692=ORIENTED_EDGE('',*,*,#4933,.T.);
#6693=ORIENTED_EDGE('',*,*,#4934,.T.);
#6694=ORIENTED_EDGE('',*,*,#4931,.F.);
#6695=ORIENTED_EDGE('',*,*,#4699,.F.);
#6696=ORIENTED_EDGE('',*,*,#4935,.T.);
#6697=ORIENTED_EDGE('',*,*,#4936,.T.);
#6698=ORIENTED_EDGE('',*,*,#4933,.F.);
#6699=ORIENTED_EDGE('',*,*,#4698,.F.);
#6700=ORIENTED_EDGE('',*,*,#4937,.T.);
#6701=ORIENTED_EDGE('',*,*,#4938,.T.);
#6702=ORIENTED_EDGE('',*,*,#4935,.F.);
#6703=ORIENTED_EDGE('',*,*,#4697,.F.);
#6704=ORIENTED_EDGE('',*,*,#4920,.T.);
#6705=ORIENTED_EDGE('',*,*,#4939,.T.);
#6706=ORIENTED_EDGE('',*,*,#4937,.F.);
#6707=ORIENTED_EDGE('',*,*,#4939,.F.);
#6708=ORIENTED_EDGE('',*,*,#4919,.F.);
#6709=ORIENTED_EDGE('',*,*,#4922,.F.);
#6710=ORIENTED_EDGE('',*,*,#4924,.F.);
#6711=ORIENTED_EDGE('',*,*,#4926,.F.);
#6712=ORIENTED_EDGE('',*,*,#4928,.F.);
#6713=ORIENTED_EDGE('',*,*,#4930,.F.);
#6714=ORIENTED_EDGE('',*,*,#4932,.F.);
#6715=ORIENTED_EDGE('',*,*,#4934,.F.);
#6716=ORIENTED_EDGE('',*,*,#4936,.F.);
#6717=ORIENTED_EDGE('',*,*,#4938,.F.);
#6718=ORIENTED_EDGE('',*,*,#4737,.F.);
#6719=ORIENTED_EDGE('',*,*,#4940,.T.);
#6720=ORIENTED_EDGE('',*,*,#4535,.F.);
#6721=ORIENTED_EDGE('',*,*,#4940,.F.);
#6722=ORIENTED_EDGE('',*,*,#4606,.F.);
#6723=ORIENTED_EDGE('',*,*,#4941,.T.);
#6724=ORIENTED_EDGE('',*,*,#4534,.F.);
#6725=ORIENTED_EDGE('',*,*,#4941,.F.);
#6726=ORIENTED_EDGE('',*,*,#4730,.F.);
#6727=ORIENTED_EDGE('',*,*,#4942,.T.);
#6728=ORIENTED_EDGE('',*,*,#4533,.F.);
#6729=ORIENTED_EDGE('',*,*,#4942,.F.);
#6730=ORIENTED_EDGE('',*,*,#4620,.F.);
#6731=ORIENTED_EDGE('',*,*,#4943,.T.);
#6732=ORIENTED_EDGE('',*,*,#4532,.F.);
#6733=ORIENTED_EDGE('',*,*,#4943,.F.);
#6734=ORIENTED_EDGE('',*,*,#4707,.F.);
#6735=ORIENTED_EDGE('',*,*,#4944,.T.);
#6736=ORIENTED_EDGE('',*,*,#4536,.F.);
#6737=ORIENTED_EDGE('',*,*,#4944,.F.);
#6738=ORIENTED_EDGE('',*,*,#4521,.F.);
#6739=ORIENTED_EDGE('',*,*,#4945,.T.);
#6740=ORIENTED_EDGE('',*,*,#4551,.F.);
#6741=ORIENTED_EDGE('',*,*,#4530,.T.);
#6742=ORIENTED_EDGE('',*,*,#4515,.F.);
#6743=ORIENTED_EDGE('',*,*,#4561,.T.);
#6744=ORIENTED_EDGE('',*,*,#4560,.F.);
#6745=ORIENTED_EDGE('',*,*,#4946,.T.);
#6746=ORIENTED_EDGE('',*,*,#4520,.F.);
#6747=ORIENTED_EDGE('',*,*,#4946,.F.);
#6748=ORIENTED_EDGE('',*,*,#4554,.F.);
#6749=ORIENTED_EDGE('',*,*,#4945,.F.);
#6750=ORIENTED_EDGE('',*,*,#4947,.T.);
#6751=ORIENTED_EDGE('',*,*,#4948,.T.);
#6752=ORIENTED_EDGE('',*,*,#4949,.T.);
#6753=ORIENTED_EDGE('',*,*,#4950,.T.);
#6754=ORIENTED_EDGE('',*,*,#4951,.T.);
#6755=ORIENTED_EDGE('',*,*,#4952,.T.);
#6756=ORIENTED_EDGE('',*,*,#4947,.F.);
#6757=ORIENTED_EDGE('',*,*,#4953,.T.);
#6758=ORIENTED_EDGE('',*,*,#4954,.T.);
#6759=ORIENTED_EDGE('',*,*,#4955,.T.);
#6760=ORIENTED_EDGE('',*,*,#4951,.F.);
#6761=ORIENTED_EDGE('',*,*,#4956,.T.);
#6762=ORIENTED_EDGE('',*,*,#4957,.T.);
#6763=ORIENTED_EDGE('',*,*,#4958,.T.);
#6764=ORIENTED_EDGE('',*,*,#4954,.F.);
#6765=ORIENTED_EDGE('',*,*,#4959,.T.);
#6766=ORIENTED_EDGE('',*,*,#4960,.T.);
#6767=ORIENTED_EDGE('',*,*,#4961,.T.);
#6768=ORIENTED_EDGE('',*,*,#4957,.F.);
#6769=ORIENTED_EDGE('',*,*,#4962,.T.);
#6770=ORIENTED_EDGE('',*,*,#4963,.T.);
#6771=ORIENTED_EDGE('',*,*,#4964,.T.);
#6772=ORIENTED_EDGE('',*,*,#4960,.F.);
#6773=ORIENTED_EDGE('',*,*,#4965,.T.);
#6774=ORIENTED_EDGE('',*,*,#4966,.T.);
#6775=ORIENTED_EDGE('',*,*,#4967,.T.);
#6776=ORIENTED_EDGE('',*,*,#4963,.F.);
#6777=ORIENTED_EDGE('',*,*,#4968,.T.);
#6778=ORIENTED_EDGE('',*,*,#4949,.F.);
#6779=ORIENTED_EDGE('',*,*,#4969,.T.);
#6780=ORIENTED_EDGE('',*,*,#4966,.F.);
#6781=ORIENTED_EDGE('',*,*,#4970,.T.);
#6782=ORIENTED_EDGE('',*,*,#4964,.F.);
#6783=ORIENTED_EDGE('',*,*,#4971,.T.);
#6784=ORIENTED_EDGE('',*,*,#4972,.F.);
#6785=ORIENTED_EDGE('',*,*,#4973,.T.);
#6786=ORIENTED_EDGE('',*,*,#4967,.F.);
#6787=ORIENTED_EDGE('',*,*,#4974,.F.);
#6788=ORIENTED_EDGE('',*,*,#4975,.F.);
#6789=ORIENTED_EDGE('',*,*,#4971,.F.);
#6790=ORIENTED_EDGE('',*,*,#4969,.F.);
#6791=ORIENTED_EDGE('',*,*,#4976,.T.);
#6792=ORIENTED_EDGE('',*,*,#4977,.F.);
#6793=ORIENTED_EDGE('',*,*,#4974,.T.);
#6794=ORIENTED_EDGE('',*,*,#4948,.F.);
#6795=ORIENTED_EDGE('',*,*,#4978,.F.);
#6796=ORIENTED_EDGE('',*,*,#4979,.F.);
#6797=ORIENTED_EDGE('',*,*,#4976,.F.);
#6798=ORIENTED_EDGE('',*,*,#4950,.F.);
#6799=ORIENTED_EDGE('',*,*,#4970,.F.);
#6800=ORIENTED_EDGE('',*,*,#4968,.F.);
#6801=ORIENTED_EDGE('',*,*,#4965,.F.);
#6802=ORIENTED_EDGE('',*,*,#4962,.F.);
#6803=ORIENTED_EDGE('',*,*,#4959,.F.);
#6804=ORIENTED_EDGE('',*,*,#4956,.F.);
#6805=ORIENTED_EDGE('',*,*,#4953,.F.);
#6806=ORIENTED_EDGE('',*,*,#4980,.T.);
#6807=ORIENTED_EDGE('',*,*,#4981,.T.);
#6808=ORIENTED_EDGE('',*,*,#4982,.T.);
#6809=ORIENTED_EDGE('',*,*,#4983,.T.);
#6810=ORIENTED_EDGE('',*,*,#4984,.T.);
#6811=ORIENTED_EDGE('',*,*,#4985,.T.);
#6812=ORIENTED_EDGE('',*,*,#4986,.T.);
#6813=ORIENTED_EDGE('',*,*,#4987,.T.);
#6814=ORIENTED_EDGE('',*,*,#4986,.F.);
#6815=ORIENTED_EDGE('',*,*,#4988,.F.);
#6816=ORIENTED_EDGE('',*,*,#4989,.F.);
#6817=ORIENTED_EDGE('',*,*,#4990,.F.);
#6818=ORIENTED_EDGE('',*,*,#4991,.F.);
#6819=ORIENTED_EDGE('',*,*,#4992,.F.);
#6820=ORIENTED_EDGE('',*,*,#4993,.F.);
#6821=ORIENTED_EDGE('',*,*,#4994,.F.);
#6822=ORIENTED_EDGE('',*,*,#4995,.F.);
#6823=ORIENTED_EDGE('',*,*,#4996,.F.);
#6824=ORIENTED_EDGE('',*,*,#4997,.T.);
#6825=ORIENTED_EDGE('',*,*,#4998,.F.);
#6826=ORIENTED_EDGE('',*,*,#4999,.F.);
#6827=ORIENTED_EDGE('',*,*,#4987,.F.);
#6828=ORIENTED_EDGE('',*,*,#4985,.F.);
#6829=ORIENTED_EDGE('',*,*,#5000,.T.);
#6830=ORIENTED_EDGE('',*,*,#5001,.T.);
#6831=ORIENTED_EDGE('',*,*,#5000,.F.);
#6832=ORIENTED_EDGE('',*,*,#5002,.T.);
#6833=ORIENTED_EDGE('',*,*,#4988,.T.);
#6834=ORIENTED_EDGE('',*,*,#5003,.T.);
#6835=ORIENTED_EDGE('',*,*,#5004,.T.);
#6836=ORIENTED_EDGE('',*,*,#5002,.F.);
#6837=ORIENTED_EDGE('',*,*,#5005,.T.);
#6838=ORIENTED_EDGE('',*,*,#5006,.T.);
#6839=ORIENTED_EDGE('',*,*,#4989,.T.);
#6840=ORIENTED_EDGE('',*,*,#5007,.T.);
#6841=ORIENTED_EDGE('',*,*,#4990,.T.);
#6842=ORIENTED_EDGE('',*,*,#5006,.F.);
#6843=ORIENTED_EDGE('',*,*,#5008,.T.);
#6844=ORIENTED_EDGE('',*,*,#5007,.F.);
#6845=ORIENTED_EDGE('',*,*,#4972,.T.);
#6846=ORIENTED_EDGE('',*,*,#5009,.T.);
#6847=ORIENTED_EDGE('',*,*,#4991,.T.);
#6848=ORIENTED_EDGE('',*,*,#5010,.T.);
#6849=ORIENTED_EDGE('',*,*,#4992,.T.);
#6850=ORIENTED_EDGE('',*,*,#5009,.F.);
#6851=ORIENTED_EDGE('',*,*,#4975,.T.);
#6852=ORIENTED_EDGE('',*,*,#5010,.F.);
#6853=ORIENTED_EDGE('',*,*,#4977,.T.);
#6854=ORIENTED_EDGE('',*,*,#5011,.T.);
#6855=ORIENTED_EDGE('',*,*,#4993,.T.);
#6856=ORIENTED_EDGE('',*,*,#5012,.T.);
#6857=ORIENTED_EDGE('',*,*,#4994,.T.);
#6858=ORIENTED_EDGE('',*,*,#5011,.F.);
#6859=ORIENTED_EDGE('',*,*,#4979,.T.);
#6860=ORIENTED_EDGE('',*,*,#5012,.F.);
#6861=ORIENTED_EDGE('',*,*,#5013,.T.);
#6862=ORIENTED_EDGE('',*,*,#5003,.F.);
#6863=ORIENTED_EDGE('',*,*,#4995,.T.);
#6864=ORIENTED_EDGE('',*,*,#4961,.F.);
#6865=ORIENTED_EDGE('',*,*,#4973,.F.);
#6866=ORIENTED_EDGE('',*,*,#5008,.F.);
#6867=ORIENTED_EDGE('',*,*,#5014,.F.);
#6868=ORIENTED_EDGE('',*,*,#4958,.F.);
#6869=ORIENTED_EDGE('',*,*,#5014,.T.);
#6870=ORIENTED_EDGE('',*,*,#5005,.F.);
#6871=ORIENTED_EDGE('',*,*,#5015,.T.);
#6872=ORIENTED_EDGE('',*,*,#4955,.F.);
#6873=ORIENTED_EDGE('',*,*,#5015,.F.);
#6874=ORIENTED_EDGE('',*,*,#5004,.F.);
#6875=ORIENTED_EDGE('',*,*,#5016,.F.);
#6876=ORIENTED_EDGE('',*,*,#5017,.T.);
#6877=ORIENTED_EDGE('',*,*,#5018,.T.);
#6878=ORIENTED_EDGE('',*,*,#4999,.T.);
#6879=ORIENTED_EDGE('',*,*,#5018,.F.);
#6880=ORIENTED_EDGE('',*,*,#5017,.F.);
#6881=ORIENTED_EDGE('',*,*,#5019,.T.);
#6882=ORIENTED_EDGE('',*,*,#5020,.T.);
#6883=ORIENTED_EDGE('',*,*,#5019,.F.);
#6884=ORIENTED_EDGE('',*,*,#5021,.T.);
#6885=ORIENTED_EDGE('',*,*,#5022,.T.);
#6886=ORIENTED_EDGE('',*,*,#4996,.T.);
#6887=ORIENTED_EDGE('',*,*,#5022,.F.);
#6888=ORIENTED_EDGE('',*,*,#5021,.F.);
#6889=ORIENTED_EDGE('',*,*,#5023,.T.);
#6890=ORIENTED_EDGE('',*,*,#5024,.T.);
#6891=ORIENTED_EDGE('',*,*,#5023,.F.);
#6892=ORIENTED_EDGE('',*,*,#5025,.T.);
#6893=ORIENTED_EDGE('',*,*,#5026,.T.);
#6894=ORIENTED_EDGE('',*,*,#4998,.T.);
#6895=ORIENTED_EDGE('',*,*,#5026,.F.);
#6896=ORIENTED_EDGE('',*,*,#5025,.F.);
#6897=ORIENTED_EDGE('',*,*,#5027,.T.);
#6898=ORIENTED_EDGE('',*,*,#5028,.T.);
#6899=ORIENTED_EDGE('',*,*,#5027,.F.);
#6900=ORIENTED_EDGE('',*,*,#5028,.F.);
#6901=ORIENTED_EDGE('',*,*,#5029,.T.);
#6902=ORIENTED_EDGE('',*,*,#4983,.F.);
#6903=ORIENTED_EDGE('',*,*,#5029,.F.);
#6904=ORIENTED_EDGE('',*,*,#5024,.F.);
#6905=ORIENTED_EDGE('',*,*,#5030,.T.);
#6906=ORIENTED_EDGE('',*,*,#4982,.F.);
#6907=ORIENTED_EDGE('',*,*,#5030,.F.);
#6908=ORIENTED_EDGE('',*,*,#5001,.F.);
#6909=ORIENTED_EDGE('',*,*,#5031,.T.);
#6910=ORIENTED_EDGE('',*,*,#4981,.F.);
#6911=ORIENTED_EDGE('',*,*,#5031,.F.);
#6912=ORIENTED_EDGE('',*,*,#5020,.F.);
#6913=ORIENTED_EDGE('',*,*,#5032,.T.);
#6914=ORIENTED_EDGE('',*,*,#4980,.F.);
#6915=ORIENTED_EDGE('',*,*,#5032,.F.);
#6916=ORIENTED_EDGE('',*,*,#4997,.F.);
#6917=ORIENTED_EDGE('',*,*,#5033,.T.);
#6918=ORIENTED_EDGE('',*,*,#4984,.F.);
#6919=ORIENTED_EDGE('',*,*,#5033,.F.);
#6920=ORIENTED_EDGE('',*,*,#4952,.F.);
#6921=ORIENTED_EDGE('',*,*,#5016,.T.);
#6922=ORIENTED_EDGE('',*,*,#5013,.F.);
#6923=ORIENTED_EDGE('',*,*,#4978,.T.);
#6924=ORIENTED_EDGE('',*,*,#5034,.T.);
#6925=ORIENTED_EDGE('',*,*,#5035,.T.);
#6926=ORIENTED_EDGE('',*,*,#5036,.T.);
#6927=ORIENTED_EDGE('',*,*,#5035,.F.);
#6928=ORIENTED_EDGE('',*,*,#5037,.F.);
#6929=ORIENTED_EDGE('',*,*,#5038,.F.);
#6930=ORIENTED_EDGE('',*,*,#5039,.F.);
#6931=ORIENTED_EDGE('',*,*,#5040,.F.);
#6932=ORIENTED_EDGE('',*,*,#5041,.F.);
#6933=ORIENTED_EDGE('',*,*,#5042,.F.);
#6934=ORIENTED_EDGE('',*,*,#5043,.F.);
#6935=ORIENTED_EDGE('',*,*,#5044,.F.);
#6936=ORIENTED_EDGE('',*,*,#5045,.F.);
#6937=ORIENTED_EDGE('',*,*,#5046,.F.);
#6938=ORIENTED_EDGE('',*,*,#5047,.F.);
#6939=ORIENTED_EDGE('',*,*,#5048,.F.);
#6940=ORIENTED_EDGE('',*,*,#5049,.F.);
#6941=ORIENTED_EDGE('',*,*,#5050,.F.);
#6942=ORIENTED_EDGE('',*,*,#5051,.F.);
#6943=ORIENTED_EDGE('',*,*,#5052,.F.);
#6944=ORIENTED_EDGE('',*,*,#5053,.F.);
#6945=ORIENTED_EDGE('',*,*,#5054,.F.);
#6946=ORIENTED_EDGE('',*,*,#5055,.F.);
#6947=ORIENTED_EDGE('',*,*,#5056,.F.);
#6948=ORIENTED_EDGE('',*,*,#5057,.F.);
#6949=ORIENTED_EDGE('',*,*,#5058,.F.);
#6950=ORIENTED_EDGE('',*,*,#5059,.T.);
#6951=ORIENTED_EDGE('',*,*,#5060,.F.);
#6952=ORIENTED_EDGE('',*,*,#5061,.F.);
#6953=ORIENTED_EDGE('',*,*,#5034,.F.);
#6954=ORIENTED_EDGE('',*,*,#5036,.F.);
#6955=ORIENTED_EDGE('',*,*,#5062,.T.);
#6956=ORIENTED_EDGE('',*,*,#5063,.T.);
#6957=ORIENTED_EDGE('',*,*,#5062,.F.);
#6958=ORIENTED_EDGE('',*,*,#5061,.T.);
#6959=ORIENTED_EDGE('',*,*,#5064,.T.);
#6960=ORIENTED_EDGE('',*,*,#5065,.T.);
#6961=ORIENTED_EDGE('',*,*,#5064,.F.);
#6962=ORIENTED_EDGE('',*,*,#5065,.F.);
#6963=ORIENTED_EDGE('',*,*,#5066,.T.);
#6964=ORIENTED_EDGE('',*,*,#5067,.T.);
#6965=ORIENTED_EDGE('',*,*,#5066,.F.);
#6966=ORIENTED_EDGE('',*,*,#5068,.T.);
#6967=ORIENTED_EDGE('',*,*,#5069,.T.);
#6968=ORIENTED_EDGE('',*,*,#5070,.T.);
#6969=ORIENTED_EDGE('',*,*,#5071,.T.);
#6970=ORIENTED_EDGE('',*,*,#5072,.T.);
#6971=ORIENTED_EDGE('',*,*,#5073,.T.);
#6972=ORIENTED_EDGE('',*,*,#5069,.F.);
#6973=ORIENTED_EDGE('',*,*,#5074,.F.);
#6974=ORIENTED_EDGE('',*,*,#5075,.F.);
#6975=ORIENTED_EDGE('',*,*,#5076,.F.);
#6976=ORIENTED_EDGE('',*,*,#5068,.F.);
#6977=ORIENTED_EDGE('',*,*,#5077,.F.);
#6978=ORIENTED_EDGE('',*,*,#5078,.T.);
#6979=ORIENTED_EDGE('',*,*,#5079,.T.);
#6980=ORIENTED_EDGE('',*,*,#5080,.F.);
#6981=ORIENTED_EDGE('',*,*,#5074,.T.);
#6982=ORIENTED_EDGE('',*,*,#5073,.F.);
#6983=ORIENTED_EDGE('',*,*,#5081,.T.);
#6984=ORIENTED_EDGE('',*,*,#5082,.T.);
#6985=ORIENTED_EDGE('',*,*,#5083,.T.);
#6986=ORIENTED_EDGE('',*,*,#5077,.T.);
#6987=ORIENTED_EDGE('',*,*,#5084,.T.);
#6988=ORIENTED_EDGE('',*,*,#5075,.T.);
#6989=ORIENTED_EDGE('',*,*,#5080,.T.);
#6990=ORIENTED_EDGE('',*,*,#5085,.T.);
#6991=ORIENTED_EDGE('',*,*,#5086,.T.);
#6992=ORIENTED_EDGE('',*,*,#5087,.T.);
#6993=ORIENTED_EDGE('',*,*,#5070,.F.);
#6994=ORIENTED_EDGE('',*,*,#5076,.T.);
#6995=ORIENTED_EDGE('',*,*,#5084,.F.);
#6996=ORIENTED_EDGE('',*,*,#5088,.F.);
#6997=ORIENTED_EDGE('',*,*,#5038,.T.);
#6998=ORIENTED_EDGE('',*,*,#5089,.F.);
#6999=ORIENTED_EDGE('',*,*,#5087,.F.);
#7000=ORIENTED_EDGE('',*,*,#5090,.T.);
#7001=ORIENTED_EDGE('',*,*,#5091,.F.);
#7002=ORIENTED_EDGE('',*,*,#5039,.T.);
#7003=ORIENTED_EDGE('',*,*,#5088,.T.);
#7004=ORIENTED_EDGE('',*,*,#5092,.T.);
#7005=ORIENTED_EDGE('',*,*,#5093,.T.);
#7006=ORIENTED_EDGE('',*,*,#5094,.T.);
#7007=ORIENTED_EDGE('',*,*,#5093,.F.);
#7008=ORIENTED_EDGE('',*,*,#5083,.F.);
#7009=ORIENTED_EDGE('',*,*,#5095,.F.);
#7010=ORIENTED_EDGE('',*,*,#5096,.T.);
#7011=ORIENTED_EDGE('',*,*,#5097,.F.);
#7012=ORIENTED_EDGE('',*,*,#5098,.F.);
#7013=ORIENTED_EDGE('',*,*,#5099,.F.);
#7014=ORIENTED_EDGE('',*,*,#5100,.F.);
#7015=ORIENTED_EDGE('',*,*,#5101,.F.);
#7016=ORIENTED_EDGE('',*,*,#5102,.F.);
#7017=ORIENTED_EDGE('',*,*,#5103,.F.);
#7018=ORIENTED_EDGE('',*,*,#5104,.F.);
#7019=ORIENTED_EDGE('',*,*,#5105,.F.);
#7020=ORIENTED_EDGE('',*,*,#5106,.F.);
#7021=ORIENTED_EDGE('',*,*,#5107,.F.);
#7022=ORIENTED_EDGE('',*,*,#5108,.F.);
#7023=ORIENTED_EDGE('',*,*,#5109,.F.);
#7024=ORIENTED_EDGE('',*,*,#5110,.F.);
#7025=ORIENTED_EDGE('',*,*,#5111,.F.);
#7026=ORIENTED_EDGE('',*,*,#5112,.F.);
#7027=ORIENTED_EDGE('',*,*,#5113,.F.);
#7028=ORIENTED_EDGE('',*,*,#5114,.F.);
#7029=ORIENTED_EDGE('',*,*,#5115,.F.);
#7030=ORIENTED_EDGE('',*,*,#5116,.F.);
#7031=ORIENTED_EDGE('',*,*,#5078,.F.);
#7032=ORIENTED_EDGE('',*,*,#5117,.F.);
#7033=ORIENTED_EDGE('',*,*,#5092,.F.);
#7034=ORIENTED_EDGE('',*,*,#5094,.F.);
#7035=ORIENTED_EDGE('',*,*,#5118,.T.);
#7036=ORIENTED_EDGE('',*,*,#5119,.T.);
#7037=ORIENTED_EDGE('',*,*,#5118,.F.);
#7038=ORIENTED_EDGE('',*,*,#5117,.T.);
#7039=ORIENTED_EDGE('',*,*,#5120,.T.);
#7040=ORIENTED_EDGE('',*,*,#5121,.T.);
#7041=ORIENTED_EDGE('',*,*,#5120,.F.);
#7042=ORIENTED_EDGE('',*,*,#5121,.F.);
#7043=ORIENTED_EDGE('',*,*,#5122,.T.);
#7044=ORIENTED_EDGE('',*,*,#5123,.T.);
#7045=ORIENTED_EDGE('',*,*,#5122,.F.);
#7046=ORIENTED_EDGE('',*,*,#5124,.F.);
#7047=ORIENTED_EDGE('',*,*,#5125,.F.);
#7048=ORIENTED_EDGE('',*,*,#5126,.F.);
#7049=ORIENTED_EDGE('',*,*,#5071,.F.);
#7050=ORIENTED_EDGE('',*,*,#5089,.T.);
#7051=ORIENTED_EDGE('',*,*,#5037,.T.);
#7052=ORIENTED_EDGE('',*,*,#5125,.T.);
#7053=ORIENTED_EDGE('',*,*,#5127,.T.);
#7054=ORIENTED_EDGE('',*,*,#5128,.T.);
#7055=ORIENTED_EDGE('',*,*,#5129,.T.);
#7056=ORIENTED_EDGE('',*,*,#5126,.T.);
#7057=ORIENTED_EDGE('',*,*,#5060,.T.);
#7058=ORIENTED_EDGE('',*,*,#5082,.F.);
#7059=ORIENTED_EDGE('',*,*,#5130,.F.);
#7060=ORIENTED_EDGE('',*,*,#5131,.F.);
#7061=ORIENTED_EDGE('',*,*,#5130,.T.);
#7062=ORIENTED_EDGE('',*,*,#5132,.T.);
#7063=ORIENTED_EDGE('',*,*,#5124,.T.);
#7064=ORIENTED_EDGE('',*,*,#5133,.T.);
#7065=ORIENTED_EDGE('',*,*,#5134,.T.);
#7066=ORIENTED_EDGE('',*,*,#5095,.T.);
#7067=ORIENTED_EDGE('',*,*,#5131,.T.);
#7068=ORIENTED_EDGE('',*,*,#5135,.T.);
#7069=ORIENTED_EDGE('',*,*,#5072,.F.);
#7070=ORIENTED_EDGE('',*,*,#5127,.F.);
#7071=ORIENTED_EDGE('',*,*,#5132,.F.);
#7072=ORIENTED_EDGE('',*,*,#5081,.F.);
#7073=ORIENTED_EDGE('',*,*,#5136,.F.);
#7074=ORIENTED_EDGE('',*,*,#5137,.F.);
#7075=ORIENTED_EDGE('',*,*,#5138,.F.);
#7076=ORIENTED_EDGE('',*,*,#5139,.T.);
#7077=ORIENTED_EDGE('',*,*,#5140,.T.);
#7078=ORIENTED_EDGE('',*,*,#5137,.T.);
#7079=ORIENTED_EDGE('',*,*,#5057,.T.);
#7080=ORIENTED_EDGE('',*,*,#5141,.T.);
#7081=ORIENTED_EDGE('',*,*,#5142,.F.);
#7082=ORIENTED_EDGE('',*,*,#5143,.F.);
#7083=ORIENTED_EDGE('',*,*,#5144,.F.);
#7084=ORIENTED_EDGE('',*,*,#5143,.T.);
#7085=ORIENTED_EDGE('',*,*,#5145,.T.);
#7086=ORIENTED_EDGE('',*,*,#5138,.T.);
#7087=ORIENTED_EDGE('',*,*,#5146,.T.);
#7088=ORIENTED_EDGE('',*,*,#5147,.T.);
#7089=ORIENTED_EDGE('',*,*,#5098,.T.);
#7090=ORIENTED_EDGE('',*,*,#5144,.T.);
#7091=ORIENTED_EDGE('',*,*,#5148,.T.);
#7092=ORIENTED_EDGE('',*,*,#5149,.T.);
#7093=ORIENTED_EDGE('',*,*,#5150,.T.);
#7094=ORIENTED_EDGE('',*,*,#5151,.T.);
#7095=ORIENTED_EDGE('',*,*,#5142,.T.);
#7096=ORIENTED_EDGE('',*,*,#5097,.T.);
#7097=ORIENTED_EDGE('',*,*,#5152,.T.);
#7098=ORIENTED_EDGE('',*,*,#5058,.T.);
#7099=ORIENTED_EDGE('',*,*,#5136,.T.);
#7100=ORIENTED_EDGE('',*,*,#5153,.T.);
#7101=ORIENTED_EDGE('',*,*,#5153,.F.);
#7102=ORIENTED_EDGE('',*,*,#5145,.F.);
#7103=ORIENTED_EDGE('',*,*,#5151,.F.);
#7104=ORIENTED_EDGE('',*,*,#5154,.T.);
#7105=ORIENTED_EDGE('',*,*,#5155,.T.);
#7106=ORIENTED_EDGE('',*,*,#5156,.T.);
#7107=ORIENTED_EDGE('',*,*,#5157,.T.);
#7108=ORIENTED_EDGE('',*,*,#5128,.F.);
#7109=ORIENTED_EDGE('',*,*,#5059,.F.);
#7110=ORIENTED_EDGE('',*,*,#5152,.F.);
#7111=ORIENTED_EDGE('',*,*,#5154,.F.);
#7112=ORIENTED_EDGE('',*,*,#5150,.F.);
#7113=ORIENTED_EDGE('',*,*,#5096,.F.);
#7114=ORIENTED_EDGE('',*,*,#5134,.F.);
#7115=ORIENTED_EDGE('',*,*,#5158,.F.);
#7116=ORIENTED_EDGE('',*,*,#5147,.F.);
#7117=ORIENTED_EDGE('',*,*,#5159,.T.);
#7118=ORIENTED_EDGE('',*,*,#5160,.F.);
#7119=ORIENTED_EDGE('',*,*,#5099,.T.);
#7120=ORIENTED_EDGE('',*,*,#5161,.T.);
#7121=ORIENTED_EDGE('',*,*,#5162,.T.);
#7122=ORIENTED_EDGE('',*,*,#5110,.T.);
#7123=ORIENTED_EDGE('',*,*,#5163,.T.);
#7124=ORIENTED_EDGE('',*,*,#5085,.F.);
#7125=ORIENTED_EDGE('',*,*,#5079,.F.);
#7126=ORIENTED_EDGE('',*,*,#5116,.T.);
#7127=ORIENTED_EDGE('',*,*,#5164,.T.);
#7128=ORIENTED_EDGE('',*,*,#5165,.T.);
#7129=ORIENTED_EDGE('',*,*,#5115,.T.);
#7130=ORIENTED_EDGE('',*,*,#5166,.T.);
#7131=ORIENTED_EDGE('',*,*,#5167,.T.);
#7132=ORIENTED_EDGE('',*,*,#5164,.F.);
#7133=ORIENTED_EDGE('',*,*,#5114,.T.);
#7134=ORIENTED_EDGE('',*,*,#5168,.T.);
#7135=ORIENTED_EDGE('',*,*,#5169,.T.);
#7136=ORIENTED_EDGE('',*,*,#5166,.F.);
#7137=ORIENTED_EDGE('',*,*,#5170,.T.);
#7138=ORIENTED_EDGE('',*,*,#5168,.F.);
#7139=ORIENTED_EDGE('',*,*,#5113,.T.);
#7140=ORIENTED_EDGE('',*,*,#5171,.T.);
#7141=ORIENTED_EDGE('',*,*,#5172,.T.);
#7142=ORIENTED_EDGE('',*,*,#5171,.F.);
#7143=ORIENTED_EDGE('',*,*,#5112,.T.);
#7144=ORIENTED_EDGE('',*,*,#5173,.T.);
#7145=ORIENTED_EDGE('',*,*,#5174,.T.);
#7146=ORIENTED_EDGE('',*,*,#5173,.F.);
#7147=ORIENTED_EDGE('',*,*,#5111,.T.);
#7148=ORIENTED_EDGE('',*,*,#5162,.F.);
#7149=ORIENTED_EDGE('',*,*,#5175,.T.);
#7150=ORIENTED_EDGE('',*,*,#5163,.F.);
#7151=ORIENTED_EDGE('',*,*,#5109,.T.);
#7152=ORIENTED_EDGE('',*,*,#5176,.T.);
#7153=ORIENTED_EDGE('',*,*,#5177,.T.);
#7154=ORIENTED_EDGE('',*,*,#5176,.F.);
#7155=ORIENTED_EDGE('',*,*,#5108,.T.);
#7156=ORIENTED_EDGE('',*,*,#5178,.T.);
#7157=ORIENTED_EDGE('',*,*,#5179,.T.);
#7158=ORIENTED_EDGE('',*,*,#5178,.F.);
#7159=ORIENTED_EDGE('',*,*,#5107,.T.);
#7160=ORIENTED_EDGE('',*,*,#5180,.T.);
#7161=ORIENTED_EDGE('',*,*,#5181,.T.);
#7162=ORIENTED_EDGE('',*,*,#5180,.F.);
#7163=ORIENTED_EDGE('',*,*,#5106,.T.);
#7164=ORIENTED_EDGE('',*,*,#5182,.T.);
#7165=ORIENTED_EDGE('',*,*,#5183,.T.);
#7166=ORIENTED_EDGE('',*,*,#5182,.F.);
#7167=ORIENTED_EDGE('',*,*,#5105,.T.);
#7168=ORIENTED_EDGE('',*,*,#5184,.T.);
#7169=ORIENTED_EDGE('',*,*,#5185,.T.);
#7170=ORIENTED_EDGE('',*,*,#5184,.F.);
#7171=ORIENTED_EDGE('',*,*,#5104,.T.);
#7172=ORIENTED_EDGE('',*,*,#5186,.T.);
#7173=ORIENTED_EDGE('',*,*,#5187,.T.);
#7174=ORIENTED_EDGE('',*,*,#5186,.F.);
#7175=ORIENTED_EDGE('',*,*,#5103,.T.);
#7176=ORIENTED_EDGE('',*,*,#5188,.T.);
#7177=ORIENTED_EDGE('',*,*,#5189,.T.);
#7178=ORIENTED_EDGE('',*,*,#5188,.F.);
#7179=ORIENTED_EDGE('',*,*,#5102,.T.);
#7180=ORIENTED_EDGE('',*,*,#5190,.T.);
#7181=ORIENTED_EDGE('',*,*,#5191,.T.);
#7182=ORIENTED_EDGE('',*,*,#5190,.F.);
#7183=ORIENTED_EDGE('',*,*,#5101,.T.);
#7184=ORIENTED_EDGE('',*,*,#5192,.T.);
#7185=ORIENTED_EDGE('',*,*,#5193,.T.);
#7186=ORIENTED_EDGE('',*,*,#5192,.F.);
#7187=ORIENTED_EDGE('',*,*,#5100,.T.);
#7188=ORIENTED_EDGE('',*,*,#5160,.T.);
#7189=ORIENTED_EDGE('',*,*,#5183,.F.);
#7190=ORIENTED_EDGE('',*,*,#5194,.T.);
#7191=ORIENTED_EDGE('',*,*,#5195,.F.);
#7192=ORIENTED_EDGE('',*,*,#5196,.T.);
#7193=ORIENTED_EDGE('',*,*,#5185,.F.);
#7194=ORIENTED_EDGE('',*,*,#5197,.F.);
#7195=ORIENTED_EDGE('',*,*,#5198,.F.);
#7196=ORIENTED_EDGE('',*,*,#5194,.F.);
#7197=ORIENTED_EDGE('',*,*,#5187,.F.);
#7198=ORIENTED_EDGE('',*,*,#5199,.F.);
#7199=ORIENTED_EDGE('',*,*,#5200,.F.);
#7200=ORIENTED_EDGE('',*,*,#5197,.T.);
#7201=ORIENTED_EDGE('',*,*,#5189,.F.);
#7202=ORIENTED_EDGE('',*,*,#5201,.F.);
#7203=ORIENTED_EDGE('',*,*,#5202,.F.);
#7204=ORIENTED_EDGE('',*,*,#5199,.T.);
#7205=ORIENTED_EDGE('',*,*,#5191,.F.);
#7206=ORIENTED_EDGE('',*,*,#5203,.T.);
#7207=ORIENTED_EDGE('',*,*,#5204,.F.);
#7208=ORIENTED_EDGE('',*,*,#5201,.T.);
#7209=ORIENTED_EDGE('',*,*,#5193,.F.);
#7210=ORIENTED_EDGE('',*,*,#5205,.F.);
#7211=ORIENTED_EDGE('',*,*,#5206,.F.);
#7212=ORIENTED_EDGE('',*,*,#5203,.F.);
#7213=ORIENTED_EDGE('',*,*,#5139,.F.);
#7214=ORIENTED_EDGE('',*,*,#5207,.F.);
#7215=ORIENTED_EDGE('',*,*,#5205,.T.);
#7216=ORIENTED_EDGE('',*,*,#5159,.F.);
#7217=ORIENTED_EDGE('',*,*,#5149,.F.);
#7218=ORIENTED_EDGE('',*,*,#5208,.T.);
#7219=ORIENTED_EDGE('',*,*,#5140,.F.);
#7220=ORIENTED_EDGE('',*,*,#5208,.F.);
#7221=ORIENTED_EDGE('',*,*,#5148,.F.);
#7222=ORIENTED_EDGE('',*,*,#5146,.F.);
#7223=ORIENTED_EDGE('',*,*,#5141,.F.);
#7224=ORIENTED_EDGE('',*,*,#5056,.T.);
#7225=ORIENTED_EDGE('',*,*,#5209,.T.);
#7226=ORIENTED_EDGE('',*,*,#5207,.T.);
#7227=ORIENTED_EDGE('',*,*,#5055,.T.);
#7228=ORIENTED_EDGE('',*,*,#5210,.T.);
#7229=ORIENTED_EDGE('',*,*,#5206,.T.);
#7230=ORIENTED_EDGE('',*,*,#5209,.F.);
#7231=ORIENTED_EDGE('',*,*,#5054,.T.);
#7232=ORIENTED_EDGE('',*,*,#5211,.T.);
#7233=ORIENTED_EDGE('',*,*,#5204,.T.);
#7234=ORIENTED_EDGE('',*,*,#5210,.F.);
#7235=ORIENTED_EDGE('',*,*,#5053,.T.);
#7236=ORIENTED_EDGE('',*,*,#5212,.T.);
#7237=ORIENTED_EDGE('',*,*,#5202,.T.);
#7238=ORIENTED_EDGE('',*,*,#5211,.F.);
#7239=ORIENTED_EDGE('',*,*,#5052,.T.);
#7240=ORIENTED_EDGE('',*,*,#5213,.T.);
#7241=ORIENTED_EDGE('',*,*,#5200,.T.);
#7242=ORIENTED_EDGE('',*,*,#5212,.F.);
#7243=ORIENTED_EDGE('',*,*,#5051,.T.);
#7244=ORIENTED_EDGE('',*,*,#5214,.T.);
#7245=ORIENTED_EDGE('',*,*,#5198,.T.);
#7246=ORIENTED_EDGE('',*,*,#5213,.F.);
#7247=ORIENTED_EDGE('',*,*,#5050,.T.);
#7248=ORIENTED_EDGE('',*,*,#5215,.T.);
#7249=ORIENTED_EDGE('',*,*,#5195,.T.);
#7250=ORIENTED_EDGE('',*,*,#5214,.F.);
#7251=ORIENTED_EDGE('',*,*,#5049,.T.);
#7252=ORIENTED_EDGE('',*,*,#5216,.T.);
#7253=ORIENTED_EDGE('',*,*,#5217,.T.);
#7254=ORIENTED_EDGE('',*,*,#5215,.F.);
#7255=ORIENTED_EDGE('',*,*,#5048,.T.);
#7256=ORIENTED_EDGE('',*,*,#5218,.T.);
#7257=ORIENTED_EDGE('',*,*,#5219,.T.);
#7258=ORIENTED_EDGE('',*,*,#5216,.F.);
#7259=ORIENTED_EDGE('',*,*,#5047,.T.);
#7260=ORIENTED_EDGE('',*,*,#5220,.T.);
#7261=ORIENTED_EDGE('',*,*,#5221,.T.);
#7262=ORIENTED_EDGE('',*,*,#5218,.F.);
#7263=ORIENTED_EDGE('',*,*,#5046,.T.);
#7264=ORIENTED_EDGE('',*,*,#5222,.T.);
#7265=ORIENTED_EDGE('',*,*,#5223,.T.);
#7266=ORIENTED_EDGE('',*,*,#5220,.F.);
#7267=ORIENTED_EDGE('',*,*,#5045,.T.);
#7268=ORIENTED_EDGE('',*,*,#5224,.T.);
#7269=ORIENTED_EDGE('',*,*,#5225,.T.);
#7270=ORIENTED_EDGE('',*,*,#5222,.F.);
#7271=ORIENTED_EDGE('',*,*,#5043,.T.);
#7272=ORIENTED_EDGE('',*,*,#5226,.T.);
#7273=ORIENTED_EDGE('',*,*,#5227,.T.);
#7274=ORIENTED_EDGE('',*,*,#5228,.T.);
#7275=ORIENTED_EDGE('',*,*,#5229,.T.);
#7276=ORIENTED_EDGE('',*,*,#5226,.F.);
#7277=ORIENTED_EDGE('',*,*,#5042,.T.);
#7278=ORIENTED_EDGE('',*,*,#5230,.T.);
#7279=ORIENTED_EDGE('',*,*,#5231,.T.);
#7280=ORIENTED_EDGE('',*,*,#5230,.F.);
#7281=ORIENTED_EDGE('',*,*,#5041,.T.);
#7282=ORIENTED_EDGE('',*,*,#5232,.T.);
#7283=ORIENTED_EDGE('',*,*,#5044,.T.);
#7284=ORIENTED_EDGE('',*,*,#5228,.F.);
#7285=ORIENTED_EDGE('',*,*,#5233,.T.);
#7286=ORIENTED_EDGE('',*,*,#5224,.F.);
#7287=ORIENTED_EDGE('',*,*,#5234,.T.);
#7288=ORIENTED_EDGE('',*,*,#5232,.F.);
#7289=ORIENTED_EDGE('',*,*,#5040,.T.);
#7290=ORIENTED_EDGE('',*,*,#5091,.T.);
#7291=ORIENTED_EDGE('',*,*,#5181,.F.);
#7292=ORIENTED_EDGE('',*,*,#5196,.F.);
#7293=ORIENTED_EDGE('',*,*,#5217,.F.);
#7294=ORIENTED_EDGE('',*,*,#5235,.F.);
#7295=ORIENTED_EDGE('',*,*,#5179,.F.);
#7296=ORIENTED_EDGE('',*,*,#5235,.T.);
#7297=ORIENTED_EDGE('',*,*,#5219,.F.);
#7298=ORIENTED_EDGE('',*,*,#5236,.T.);
#7299=ORIENTED_EDGE('',*,*,#5177,.F.);
#7300=ORIENTED_EDGE('',*,*,#5236,.F.);
#7301=ORIENTED_EDGE('',*,*,#5221,.F.);
#7302=ORIENTED_EDGE('',*,*,#5237,.F.);
#7303=ORIENTED_EDGE('',*,*,#5238,.T.);
#7304=ORIENTED_EDGE('',*,*,#5239,.T.);
#7305=ORIENTED_EDGE('',*,*,#5240,.T.);
#7306=ORIENTED_EDGE('',*,*,#5175,.F.);
#7307=ORIENTED_EDGE('',*,*,#5237,.T.);
#7308=ORIENTED_EDGE('',*,*,#5223,.F.);
#7309=ORIENTED_EDGE('',*,*,#5241,.T.);
#7310=ORIENTED_EDGE('',*,*,#5161,.F.);
#7311=ORIENTED_EDGE('',*,*,#5241,.F.);
#7312=ORIENTED_EDGE('',*,*,#5225,.F.);
#7313=ORIENTED_EDGE('',*,*,#5242,.T.);
#7314=ORIENTED_EDGE('',*,*,#5174,.F.);
#7315=ORIENTED_EDGE('',*,*,#5242,.F.);
#7316=ORIENTED_EDGE('',*,*,#5233,.F.);
#7317=ORIENTED_EDGE('',*,*,#5243,.T.);
#7318=ORIENTED_EDGE('',*,*,#5172,.F.);
#7319=ORIENTED_EDGE('',*,*,#5243,.F.);
#7320=ORIENTED_EDGE('',*,*,#5227,.F.);
#7321=ORIENTED_EDGE('',*,*,#5244,.F.);
#7322=ORIENTED_EDGE('',*,*,#5170,.F.);
#7323=ORIENTED_EDGE('',*,*,#5244,.T.);
#7324=ORIENTED_EDGE('',*,*,#5229,.F.);
#7325=ORIENTED_EDGE('',*,*,#5245,.T.);
#7326=ORIENTED_EDGE('',*,*,#5169,.F.);
#7327=ORIENTED_EDGE('',*,*,#5245,.F.);
#7328=ORIENTED_EDGE('',*,*,#5231,.F.);
#7329=ORIENTED_EDGE('',*,*,#5246,.F.);
#7330=ORIENTED_EDGE('',*,*,#5167,.F.);
#7331=ORIENTED_EDGE('',*,*,#5246,.T.);
#7332=ORIENTED_EDGE('',*,*,#5234,.F.);
#7333=ORIENTED_EDGE('',*,*,#5247,.T.);
#7334=ORIENTED_EDGE('',*,*,#5086,.F.);
#7335=ORIENTED_EDGE('',*,*,#5165,.F.);
#7336=ORIENTED_EDGE('',*,*,#5247,.F.);
#7337=ORIENTED_EDGE('',*,*,#5090,.F.);
#7338=ORIENTED_EDGE('',*,*,#5119,.F.);
#7339=ORIENTED_EDGE('',*,*,#5123,.F.);
#7340=ORIENTED_EDGE('',*,*,#5067,.F.);
#7341=ORIENTED_EDGE('',*,*,#5063,.F.);
#7342=ORIENTED_EDGE('',*,*,#5238,.F.);
#7343=ORIENTED_EDGE('',*,*,#5248,.T.);
#7344=ORIENTED_EDGE('',*,*,#5157,.F.);
#7345=ORIENTED_EDGE('',*,*,#5248,.F.);
#7346=ORIENTED_EDGE('',*,*,#5239,.F.);
#7347=ORIENTED_EDGE('',*,*,#5249,.T.);
#7348=ORIENTED_EDGE('',*,*,#5156,.F.);
#7349=ORIENTED_EDGE('',*,*,#5249,.F.);
#7350=ORIENTED_EDGE('',*,*,#5240,.F.);
#7351=ORIENTED_EDGE('',*,*,#5250,.T.);
#7352=ORIENTED_EDGE('',*,*,#5155,.F.);
#7353=ORIENTED_EDGE('',*,*,#5250,.F.);
#7354=ORIENTED_EDGE('',*,*,#5129,.F.);
#7355=ORIENTED_EDGE('',*,*,#5158,.T.);
#7356=ORIENTED_EDGE('',*,*,#5135,.F.);
#7357=ORIENTED_EDGE('',*,*,#5133,.F.);
#7358=ORIENTED_EDGE('',*,*,#5251,.F.);
#7359=ORIENTED_EDGE('',*,*,#5252,.F.);
#7360=ORIENTED_EDGE('',*,*,#5253,.T.);
#7361=ORIENTED_EDGE('',*,*,#5251,.T.);
#7362=ORIENTED_EDGE('',*,*,#5253,.F.);
#7363=ORIENTED_EDGE('',*,*,#5254,.F.);
#7364=ORIENTED_EDGE('',*,*,#5255,.T.);
#7365=ORIENTED_EDGE('',*,*,#5252,.T.);
#7366=ORIENTED_EDGE('',*,*,#5255,.F.);
#7367=ORIENTED_EDGE('',*,*,#5256,.F.);
#7368=ORIENTED_EDGE('',*,*,#5257,.T.);
#7369=ORIENTED_EDGE('',*,*,#5254,.T.);
#7370=ORIENTED_EDGE('',*,*,#5257,.F.);
#7371=ORIENTED_EDGE('',*,*,#5256,.T.);
#7372=ORIENTED_EDGE('',*,*,#5258,.T.);
#7373=ORIENTED_EDGE('',*,*,#5259,.T.);
#7374=ORIENTED_EDGE('',*,*,#5260,.T.);
#7375=ORIENTED_EDGE('',*,*,#5261,.T.);
#7376=ORIENTED_EDGE('',*,*,#5259,.F.);
#7377=ORIENTED_EDGE('',*,*,#5260,.F.);
#7378=ORIENTED_EDGE('',*,*,#5261,.F.);
#7379=ORIENTED_EDGE('',*,*,#5262,.T.);
#7380=ORIENTED_EDGE('',*,*,#5263,.T.);
#7381=ORIENTED_EDGE('',*,*,#5262,.F.);
#7382=ORIENTED_EDGE('',*,*,#5258,.F.);
#7383=ORIENTED_EDGE('',*,*,#5264,.T.);
#7384=ORIENTED_EDGE('',*,*,#5265,.T.);
#7385=ORIENTED_EDGE('',*,*,#5266,.T.);
#7386=ORIENTED_EDGE('',*,*,#5267,.T.);
#7387=ORIENTED_EDGE('',*,*,#5266,.F.);
#7388=ORIENTED_EDGE('',*,*,#5268,.T.);
#7389=ORIENTED_EDGE('',*,*,#5264,.F.);
#7390=ORIENTED_EDGE('',*,*,#5269,.F.);
#7391=ORIENTED_EDGE('',*,*,#5270,.F.);
#7392=ORIENTED_EDGE('',*,*,#5265,.F.);
#7393=ORIENTED_EDGE('',*,*,#5268,.F.);
#7394=ORIENTED_EDGE('',*,*,#5271,.F.);
#7395=ORIENTED_EDGE('',*,*,#5272,.F.);
#7396=ORIENTED_EDGE('',*,*,#5267,.F.);
#7397=ORIENTED_EDGE('',*,*,#5273,.F.);
#7398=ORIENTED_EDGE('',*,*,#5272,.T.);
#7399=ORIENTED_EDGE('',*,*,#5274,.F.);
#7400=ORIENTED_EDGE('',*,*,#5275,.F.);
#7401=ORIENTED_EDGE('',*,*,#5276,.T.);
#7402=ORIENTED_EDGE('',*,*,#5269,.T.);
#7403=ORIENTED_EDGE('',*,*,#5274,.T.);
#7404=ORIENTED_EDGE('',*,*,#5271,.T.);
#7405=ORIENTED_EDGE('',*,*,#5273,.T.);
#7406=ORIENTED_EDGE('',*,*,#5270,.T.);
#7407=ORIENTED_EDGE('',*,*,#5276,.F.);
#7408=ORIENTED_EDGE('',*,*,#5277,.F.);
#7409=ORIENTED_EDGE('',*,*,#5275,.T.);
#7410=ORIENTED_EDGE('',*,*,#5263,.F.);
#7411=ORIENTED_EDGE('',*,*,#5278,.T.);
#7412=ORIENTED_EDGE('',*,*,#5277,.T.);
#7413=ORIENTED_EDGE('',*,*,#5278,.F.);
#7414=ORIENTED_EDGE('',*,*,#5279,.T.);
#7415=ORIENTED_EDGE('',*,*,#5280,.T.);
#7416=ORIENTED_EDGE('',*,*,#5281,.T.);
#7417=ORIENTED_EDGE('',*,*,#5282,.T.);
#7418=ORIENTED_EDGE('',*,*,#5281,.F.);
#7419=ORIENTED_EDGE('',*,*,#5282,.F.);
#7420=ORIENTED_EDGE('',*,*,#5283,.F.);
#7421=ORIENTED_EDGE('',*,*,#5284,.T.);
#7422=ORIENTED_EDGE('',*,*,#5279,.F.);
#7423=ORIENTED_EDGE('',*,*,#5280,.F.);
#7424=ORIENTED_EDGE('',*,*,#5284,.F.);
#7425=ORIENTED_EDGE('',*,*,#5285,.F.);
#7426=ORIENTED_EDGE('',*,*,#5286,.T.);
#7427=ORIENTED_EDGE('',*,*,#5283,.T.);
#7428=ORIENTED_EDGE('',*,*,#5286,.F.);
#7429=ORIENTED_EDGE('',*,*,#5285,.T.);
#7430=ORIENTED_EDGE('',*,*,#5287,.F.);
#7431=ORIENTED_EDGE('',*,*,#5288,.F.);
#7432=ORIENTED_EDGE('',*,*,#5289,.T.);
#7433=ORIENTED_EDGE('',*,*,#5287,.T.);
#7434=ORIENTED_EDGE('',*,*,#5289,.F.);
#7435=ORIENTED_EDGE('',*,*,#5290,.F.);
#7436=ORIENTED_EDGE('',*,*,#5291,.T.);
#7437=ORIENTED_EDGE('',*,*,#5288,.T.);
#7438=ORIENTED_EDGE('',*,*,#5291,.F.);
#7439=ORIENTED_EDGE('',*,*,#5290,.T.);
#7440=ORIENTED_EDGE('',*,*,#5292,.T.);
#7441=ORIENTED_EDGE('',*,*,#5293,.T.);
#7442=ORIENTED_EDGE('',*,*,#5294,.T.);
#7443=ORIENTED_EDGE('',*,*,#5295,.T.);
#7444=ORIENTED_EDGE('',*,*,#5294,.F.);
#7445=ORIENTED_EDGE('',*,*,#5295,.F.);
#7446=ORIENTED_EDGE('',*,*,#5296,.T.);
#7447=ORIENTED_EDGE('',*,*,#5297,.F.);
#7448=ORIENTED_EDGE('',*,*,#5298,.T.);
#7449=ORIENTED_EDGE('',*,*,#5292,.F.);
#7450=ORIENTED_EDGE('',*,*,#5293,.F.);
#7451=ORIENTED_EDGE('',*,*,#5298,.F.);
#7452=ORIENTED_EDGE('',*,*,#5299,.T.);
#7453=ORIENTED_EDGE('',*,*,#5300,.T.);
#7454=ORIENTED_EDGE('',*,*,#5296,.F.);
#7455=ORIENTED_EDGE('',*,*,#5300,.F.);
#7456=ORIENTED_EDGE('',*,*,#5297,.T.);
#7457=ORIENTED_EDGE('',*,*,#5301,.F.);
#7458=ORIENTED_EDGE('',*,*,#5302,.F.);
#7459=ORIENTED_EDGE('',*,*,#5303,.T.);
#7460=ORIENTED_EDGE('',*,*,#5301,.T.);
#7461=ORIENTED_EDGE('',*,*,#5303,.F.);
#7462=ORIENTED_EDGE('',*,*,#5302,.T.);
#7463=ORIENTED_EDGE('',*,*,#5299,.F.);
#7464=ORIENTED_EDGE('',*,*,#5304,.T.);
#7465=ORIENTED_EDGE('',*,*,#5305,.T.);
#7466=ORIENTED_EDGE('',*,*,#5306,.F.);
#7467=ORIENTED_EDGE('',*,*,#5307,.T.);
#7468=ORIENTED_EDGE('',*,*,#5304,.F.);
#7469=ORIENTED_EDGE('',*,*,#5308,.T.);
#7470=ORIENTED_EDGE('',*,*,#5309,.F.);
#7471=ORIENTED_EDGE('',*,*,#5310,.T.);
#7472=ORIENTED_EDGE('',*,*,#5307,.F.);
#7473=ORIENTED_EDGE('',*,*,#5311,.F.);
#7474=ORIENTED_EDGE('',*,*,#5312,.F.);
#7475=ORIENTED_EDGE('',*,*,#5313,.F.);
#7476=ORIENTED_EDGE('',*,*,#5314,.T.);
#7477=ORIENTED_EDGE('',*,*,#5308,.F.);
#7478=ORIENTED_EDGE('',*,*,#5315,.T.);
#7479=ORIENTED_EDGE('',*,*,#5316,.T.);
#7480=ORIENTED_EDGE('',*,*,#5317,.F.);
#7481=ORIENTED_EDGE('',*,*,#5312,.T.);
#7482=ORIENTED_EDGE('',*,*,#5306,.T.);
#7483=ORIENTED_EDGE('',*,*,#5318,.T.);
#7484=ORIENTED_EDGE('',*,*,#5315,.F.);
#7485=ORIENTED_EDGE('',*,*,#5311,.T.);
#7486=ORIENTED_EDGE('',*,*,#5319,.T.);
#7487=ORIENTED_EDGE('',*,*,#5320,.T.);
#7488=ORIENTED_EDGE('',*,*,#5321,.F.);
#7489=ORIENTED_EDGE('',*,*,#5322,.T.);
#7490=ORIENTED_EDGE('',*,*,#5319,.F.);
#7491=ORIENTED_EDGE('',*,*,#5323,.T.);
#7492=ORIENTED_EDGE('',*,*,#5324,.T.);
#7493=ORIENTED_EDGE('',*,*,#5325,.T.);
#7494=ORIENTED_EDGE('',*,*,#5322,.F.);
#7495=ORIENTED_EDGE('',*,*,#5326,.F.);
#7496=ORIENTED_EDGE('',*,*,#5327,.T.);
#7497=ORIENTED_EDGE('',*,*,#5328,.F.);
#7498=ORIENTED_EDGE('',*,*,#5329,.F.);
#7499=ORIENTED_EDGE('',*,*,#5323,.F.);
#7500=ORIENTED_EDGE('',*,*,#5330,.T.);
#7501=ORIENTED_EDGE('',*,*,#5331,.T.);
#7502=ORIENTED_EDGE('',*,*,#5324,.F.);
#7503=ORIENTED_EDGE('',*,*,#5329,.T.);
#7504=ORIENTED_EDGE('',*,*,#5330,.F.);
#7505=ORIENTED_EDGE('',*,*,#5328,.T.);
#7506=ORIENTED_EDGE('',*,*,#5332,.F.);
#7507=ORIENTED_EDGE('',*,*,#5333,.T.);
#7508=ORIENTED_EDGE('',*,*,#5334,.T.);
#7509=ORIENTED_EDGE('',*,*,#5335,.T.);
#7510=ORIENTED_EDGE('',*,*,#5334,.F.);
#7511=ORIENTED_EDGE('',*,*,#5336,.T.);
#7512=ORIENTED_EDGE('',*,*,#5335,.F.);
#7513=ORIENTED_EDGE('',*,*,#5337,.T.);
#7514=ORIENTED_EDGE('',*,*,#5338,.F.);
#7515=ORIENTED_EDGE('',*,*,#5339,.F.);
#7516=ORIENTED_EDGE('',*,*,#5337,.F.);
#7517=ORIENTED_EDGE('',*,*,#5340,.F.);
#7518=ORIENTED_EDGE('',*,*,#5309,.T.);
#7519=ORIENTED_EDGE('',*,*,#5314,.F.);
#7520=ORIENTED_EDGE('',*,*,#5341,.F.);
#7521=ORIENTED_EDGE('',*,*,#5342,.F.);
#7522=ORIENTED_EDGE('',*,*,#5343,.F.);
#7523=ORIENTED_EDGE('',*,*,#5344,.T.);
#7524=ORIENTED_EDGE('',*,*,#5345,.T.);
#7525=ORIENTED_EDGE('',*,*,#5344,.F.);
#7526=ORIENTED_EDGE('',*,*,#5346,.F.);
#7527=ORIENTED_EDGE('',*,*,#5347,.F.);
#7528=ORIENTED_EDGE('',*,*,#5332,.T.);
#7529=ORIENTED_EDGE('',*,*,#5327,.F.);
#7530=ORIENTED_EDGE('',*,*,#5348,.F.);
#7531=ORIENTED_EDGE('',*,*,#5349,.F.);
#7532=ORIENTED_EDGE('',*,*,#5350,.F.);
#7533=ORIENTED_EDGE('',*,*,#5336,.F.);
#7534=ORIENTED_EDGE('',*,*,#5351,.F.);
#7535=ORIENTED_EDGE('',*,*,#5352,.F.);
#7536=ORIENTED_EDGE('',*,*,#5353,.F.);
#7537=ORIENTED_EDGE('',*,*,#5354,.F.);
#7538=ORIENTED_EDGE('',*,*,#5355,.F.);
#7539=ORIENTED_EDGE('',*,*,#5356,.F.);
#7540=ORIENTED_EDGE('',*,*,#5357,.F.);
#7541=ORIENTED_EDGE('',*,*,#5358,.F.);
#7542=ORIENTED_EDGE('',*,*,#5353,.T.);
#7543=ORIENTED_EDGE('',*,*,#5359,.F.);
#7544=ORIENTED_EDGE('',*,*,#5360,.F.);
#7545=ORIENTED_EDGE('',*,*,#5361,.F.);
#7546=ORIENTED_EDGE('',*,*,#5362,.F.);
#7547=ORIENTED_EDGE('',*,*,#5363,.F.);
#7548=ORIENTED_EDGE('',*,*,#5364,.F.);
#7549=ORIENTED_EDGE('',*,*,#5365,.F.);
#7550=ORIENTED_EDGE('',*,*,#5360,.T.);
#7551=ORIENTED_EDGE('',*,*,#5366,.F.);
#7552=ORIENTED_EDGE('',*,*,#5367,.F.);
#7553=ORIENTED_EDGE('',*,*,#5368,.F.);
#7554=ORIENTED_EDGE('',*,*,#5369,.F.);
#7555=ORIENTED_EDGE('',*,*,#5370,.F.);
#7556=ORIENTED_EDGE('',*,*,#5371,.F.);
#7557=ORIENTED_EDGE('',*,*,#5372,.F.);
#7558=ORIENTED_EDGE('',*,*,#5367,.T.);
#7559=ORIENTED_EDGE('',*,*,#5373,.F.);
#7560=ORIENTED_EDGE('',*,*,#5374,.F.);
#7561=ORIENTED_EDGE('',*,*,#5375,.F.);
#7562=ORIENTED_EDGE('',*,*,#5376,.F.);
#7563=ORIENTED_EDGE('',*,*,#5377,.F.);
#7564=ORIENTED_EDGE('',*,*,#5378,.F.);
#7565=ORIENTED_EDGE('',*,*,#5379,.F.);
#7566=ORIENTED_EDGE('',*,*,#5374,.T.);
#7567=ORIENTED_EDGE('',*,*,#5380,.F.);
#7568=ORIENTED_EDGE('',*,*,#5381,.F.);
#7569=ORIENTED_EDGE('',*,*,#5382,.F.);
#7570=ORIENTED_EDGE('',*,*,#5383,.F.);
#7571=ORIENTED_EDGE('',*,*,#5384,.F.);
#7572=ORIENTED_EDGE('',*,*,#5385,.F.);
#7573=ORIENTED_EDGE('',*,*,#5386,.F.);
#7574=ORIENTED_EDGE('',*,*,#5381,.T.);
#7575=ORIENTED_EDGE('',*,*,#5387,.F.);
#7576=ORIENTED_EDGE('',*,*,#5388,.T.);
#7577=ORIENTED_EDGE('',*,*,#5389,.F.);
#7578=ORIENTED_EDGE('',*,*,#5390,.F.);
#7579=ORIENTED_EDGE('',*,*,#5391,.F.);
#7580=ORIENTED_EDGE('',*,*,#5392,.F.);
#7581=ORIENTED_EDGE('',*,*,#5393,.F.);
#7582=ORIENTED_EDGE('',*,*,#5388,.F.);
#7583=ORIENTED_EDGE('',*,*,#5394,.F.);
#7584=ORIENTED_EDGE('',*,*,#5395,.T.);
#7585=ORIENTED_EDGE('',*,*,#5396,.F.);
#7586=ORIENTED_EDGE('',*,*,#5397,.F.);
#7587=ORIENTED_EDGE('',*,*,#5398,.F.);
#7588=ORIENTED_EDGE('',*,*,#5399,.F.);
#7589=ORIENTED_EDGE('',*,*,#5400,.F.);
#7590=ORIENTED_EDGE('',*,*,#5395,.F.);
#7591=ORIENTED_EDGE('',*,*,#5401,.F.);
#7592=ORIENTED_EDGE('',*,*,#5402,.F.);
#7593=ORIENTED_EDGE('',*,*,#5403,.F.);
#7594=ORIENTED_EDGE('',*,*,#5404,.F.);
#7595=ORIENTED_EDGE('',*,*,#5405,.F.);
#7596=ORIENTED_EDGE('',*,*,#5406,.F.);
#7597=ORIENTED_EDGE('',*,*,#5407,.F.);
#7598=ORIENTED_EDGE('',*,*,#5402,.T.);
#7599=ORIENTED_EDGE('',*,*,#5408,.F.);
#7600=ORIENTED_EDGE('',*,*,#5409,.F.);
#7601=ORIENTED_EDGE('',*,*,#5410,.F.);
#7602=ORIENTED_EDGE('',*,*,#5411,.F.);
#7603=ORIENTED_EDGE('',*,*,#5412,.F.);
#7604=ORIENTED_EDGE('',*,*,#5413,.F.);
#7605=ORIENTED_EDGE('',*,*,#5414,.F.);
#7606=ORIENTED_EDGE('',*,*,#5409,.T.);
#7607=ORIENTED_EDGE('',*,*,#5415,.F.);
#7608=ORIENTED_EDGE('',*,*,#5416,.T.);
#7609=ORIENTED_EDGE('',*,*,#5417,.F.);
#7610=ORIENTED_EDGE('',*,*,#5418,.F.);
#7611=ORIENTED_EDGE('',*,*,#5419,.F.);
#7612=ORIENTED_EDGE('',*,*,#5420,.F.);
#7613=ORIENTED_EDGE('',*,*,#5421,.F.);
#7614=ORIENTED_EDGE('',*,*,#5416,.F.);
#7615=ORIENTED_EDGE('',*,*,#5422,.F.);
#7616=ORIENTED_EDGE('',*,*,#5423,.F.);
#7617=ORIENTED_EDGE('',*,*,#5424,.F.);
#7618=ORIENTED_EDGE('',*,*,#5425,.F.);
#7619=ORIENTED_EDGE('',*,*,#5426,.F.);
#7620=ORIENTED_EDGE('',*,*,#5427,.F.);
#7621=ORIENTED_EDGE('',*,*,#5428,.F.);
#7622=ORIENTED_EDGE('',*,*,#5423,.T.);
#7623=ORIENTED_EDGE('',*,*,#5429,.F.);
#7624=ORIENTED_EDGE('',*,*,#5430,.F.);
#7625=ORIENTED_EDGE('',*,*,#5431,.F.);
#7626=ORIENTED_EDGE('',*,*,#5432,.F.);
#7627=ORIENTED_EDGE('',*,*,#5433,.F.);
#7628=ORIENTED_EDGE('',*,*,#5434,.F.);
#7629=ORIENTED_EDGE('',*,*,#5435,.F.);
#7630=ORIENTED_EDGE('',*,*,#5430,.T.);
#7631=ORIENTED_EDGE('',*,*,#5436,.F.);
#7632=ORIENTED_EDGE('',*,*,#5437,.T.);
#7633=ORIENTED_EDGE('',*,*,#5438,.F.);
#7634=ORIENTED_EDGE('',*,*,#5439,.F.);
#7635=ORIENTED_EDGE('',*,*,#5440,.F.);
#7636=ORIENTED_EDGE('',*,*,#5441,.F.);
#7637=ORIENTED_EDGE('',*,*,#5442,.F.);
#7638=ORIENTED_EDGE('',*,*,#5437,.F.);
#7639=ORIENTED_EDGE('',*,*,#5389,.T.);
#7640=ORIENTED_EDGE('',*,*,#5393,.T.);
#7641=ORIENTED_EDGE('',*,*,#5443,.T.);
#7642=ORIENTED_EDGE('',*,*,#5444,.T.);
#7643=ORIENTED_EDGE('',*,*,#5445,.T.);
#7644=ORIENTED_EDGE('',*,*,#5446,.F.);
#7645=ORIENTED_EDGE('',*,*,#5417,.T.);
#7646=ORIENTED_EDGE('',*,*,#5421,.T.);
#7647=ORIENTED_EDGE('',*,*,#5447,.T.);
#7648=ORIENTED_EDGE('',*,*,#5396,.T.);
#7649=ORIENTED_EDGE('',*,*,#5400,.T.);
#7650=ORIENTED_EDGE('',*,*,#5448,.T.);
#7651=ORIENTED_EDGE('',*,*,#5363,.T.);
#7652=ORIENTED_EDGE('',*,*,#5359,.T.);
#7653=ORIENTED_EDGE('',*,*,#5449,.T.);
#7654=ORIENTED_EDGE('',*,*,#5450,.T.);
#7655=ORIENTED_EDGE('',*,*,#5451,.T.);
#7656=ORIENTED_EDGE('',*,*,#5444,.F.);
#7657=ORIENTED_EDGE('',*,*,#5452,.T.);
#7658=ORIENTED_EDGE('',*,*,#5405,.T.);
#7659=ORIENTED_EDGE('',*,*,#5401,.T.);
#7660=ORIENTED_EDGE('',*,*,#5453,.T.);
#7661=ORIENTED_EDGE('',*,*,#5384,.T.);
#7662=ORIENTED_EDGE('',*,*,#5380,.T.);
#7663=ORIENTED_EDGE('',*,*,#5454,.T.);
#7664=ORIENTED_EDGE('',*,*,#5412,.T.);
#7665=ORIENTED_EDGE('',*,*,#5408,.T.);
#7666=ORIENTED_EDGE('',*,*,#5455,.T.);
#7667=ORIENTED_EDGE('',*,*,#5377,.T.);
#7668=ORIENTED_EDGE('',*,*,#5373,.T.);
#7669=ORIENTED_EDGE('',*,*,#5456,.T.);
#7670=ORIENTED_EDGE('',*,*,#5370,.T.);
#7671=ORIENTED_EDGE('',*,*,#5366,.T.);
#7672=ORIENTED_EDGE('',*,*,#5457,.T.);
#7673=ORIENTED_EDGE('',*,*,#5426,.T.);
#7674=ORIENTED_EDGE('',*,*,#5422,.T.);
#7675=ORIENTED_EDGE('',*,*,#5458,.T.);
#7676=ORIENTED_EDGE('',*,*,#5355,.T.);
#7677=ORIENTED_EDGE('',*,*,#5459,.F.);
#7678=ORIENTED_EDGE('',*,*,#5439,.T.);
#7679=ORIENTED_EDGE('',*,*,#5460,.F.);
#7680=ORIENTED_EDGE('',*,*,#5362,.T.);
#7681=ORIENTED_EDGE('',*,*,#5461,.F.);
#7682=ORIENTED_EDGE('',*,*,#5462,.F.);
#7683=ORIENTED_EDGE('',*,*,#5434,.T.);
#7684=ORIENTED_EDGE('',*,*,#5463,.F.);
#7685=ORIENTED_EDGE('',*,*,#5449,.F.);
#7686=ORIENTED_EDGE('',*,*,#5369,.T.);
#7687=ORIENTED_EDGE('',*,*,#5464,.F.);
#7688=ORIENTED_EDGE('',*,*,#5427,.T.);
#7689=ORIENTED_EDGE('',*,*,#5457,.F.);
#7690=ORIENTED_EDGE('',*,*,#5383,.T.);
#7691=ORIENTED_EDGE('',*,*,#5465,.F.);
#7692=ORIENTED_EDGE('',*,*,#5413,.T.);
#7693=ORIENTED_EDGE('',*,*,#5454,.F.);
#7694=ORIENTED_EDGE('',*,*,#5397,.T.);
#7695=ORIENTED_EDGE('',*,*,#5447,.F.);
#7696=ORIENTED_EDGE('',*,*,#5420,.T.);
#7697=ORIENTED_EDGE('',*,*,#5466,.F.);
#7698=ORIENTED_EDGE('',*,*,#5390,.T.);
#7699=ORIENTED_EDGE('',*,*,#5448,.F.);
#7700=ORIENTED_EDGE('',*,*,#5399,.T.);
#7701=ORIENTED_EDGE('',*,*,#5467,.F.);
#7702=ORIENTED_EDGE('',*,*,#5392,.T.);
#7703=ORIENTED_EDGE('',*,*,#5468,.F.);
#7704=ORIENTED_EDGE('',*,*,#5469,.F.);
#7705=ORIENTED_EDGE('',*,*,#5406,.T.);
#7706=ORIENTED_EDGE('',*,*,#5452,.F.);
#7707=ORIENTED_EDGE('',*,*,#5443,.F.);
#7708=ORIENTED_EDGE('',*,*,#5385,.T.);
#7709=ORIENTED_EDGE('',*,*,#5453,.F.);
#7710=ORIENTED_EDGE('',*,*,#5404,.T.);
#7711=ORIENTED_EDGE('',*,*,#5470,.F.);
#7712=ORIENTED_EDGE('',*,*,#5378,.T.);
#7713=ORIENTED_EDGE('',*,*,#5455,.F.);
#7714=ORIENTED_EDGE('',*,*,#5411,.T.);
#7715=ORIENTED_EDGE('',*,*,#5471,.F.);
#7716=ORIENTED_EDGE('',*,*,#5371,.T.);
#7717=ORIENTED_EDGE('',*,*,#5456,.F.);
#7718=ORIENTED_EDGE('',*,*,#5376,.T.);
#7719=ORIENTED_EDGE('',*,*,#5472,.F.);
#7720=ORIENTED_EDGE('',*,*,#5364,.T.);
#7721=ORIENTED_EDGE('',*,*,#5458,.F.);
#7722=ORIENTED_EDGE('',*,*,#5425,.T.);
#7723=ORIENTED_EDGE('',*,*,#5473,.F.);
#7724=ORIENTED_EDGE('',*,*,#5356,.T.);
#7725=ORIENTED_EDGE('',*,*,#5352,.T.);
#7726=ORIENTED_EDGE('',*,*,#5460,.T.);
#7727=ORIENTED_EDGE('',*,*,#5438,.T.);
#7728=ORIENTED_EDGE('',*,*,#5442,.T.);
#7729=ORIENTED_EDGE('',*,*,#5474,.T.);
#7730=ORIENTED_EDGE('',*,*,#5475,.T.);
#7731=ORIENTED_EDGE('',*,*,#5450,.F.);
#7732=ORIENTED_EDGE('',*,*,#5463,.T.);
#7733=ORIENTED_EDGE('',*,*,#5433,.T.);
#7734=ORIENTED_EDGE('',*,*,#5429,.T.);
#7735=ORIENTED_EDGE('',*,*,#5476,.T.);
#7736=ORIENTED_EDGE('',*,*,#5342,.T.);
#7737=ORIENTED_EDGE('',*,*,#5477,.T.);
#7738=ORIENTED_EDGE('',*,*,#5347,.T.);
#7739=ORIENTED_EDGE('',*,*,#5478,.T.);
#7740=ORIENTED_EDGE('',*,*,#5477,.F.);
#7741=ORIENTED_EDGE('',*,*,#5479,.F.);
#7742=ORIENTED_EDGE('',*,*,#5480,.F.);
#7743=ORIENTED_EDGE('',*,*,#5481,.F.);
#7744=ORIENTED_EDGE('',*,*,#5482,.F.);
#7745=ORIENTED_EDGE('',*,*,#5333,.F.);
#7746=ORIENTED_EDGE('',*,*,#5349,.T.);
#7747=ORIENTED_EDGE('',*,*,#5483,.T.);
#7748=ORIENTED_EDGE('',*,*,#5340,.T.);
#7749=ORIENTED_EDGE('',*,*,#5484,.T.);
#7750=ORIENTED_EDGE('',*,*,#5483,.F.);
#7751=ORIENTED_EDGE('',*,*,#5485,.F.);
#7752=ORIENTED_EDGE('',*,*,#5486,.F.);
#7753=ORIENTED_EDGE('',*,*,#5487,.F.);
#7754=ORIENTED_EDGE('',*,*,#5488,.F.);
#7755=ORIENTED_EDGE('',*,*,#5310,.F.);
#7756=ORIENTED_EDGE('',*,*,#5331,.F.);
#7757=ORIENTED_EDGE('',*,*,#5482,.T.);
#7758=ORIENTED_EDGE('',*,*,#5445,.F.);
#7759=ORIENTED_EDGE('',*,*,#5489,.T.);
#7760=ORIENTED_EDGE('',*,*,#5317,.T.);
#7761=ORIENTED_EDGE('',*,*,#5479,.T.);
#7762=ORIENTED_EDGE('',*,*,#5341,.T.);
#7763=ORIENTED_EDGE('',*,*,#5313,.T.);
#7764=ORIENTED_EDGE('',*,*,#5316,.F.);
#7765=ORIENTED_EDGE('',*,*,#5490,.T.);
#7766=ORIENTED_EDGE('',*,*,#5491,.F.);
#7767=ORIENTED_EDGE('',*,*,#5480,.T.);
#7768=ORIENTED_EDGE('',*,*,#5321,.T.);
#7769=ORIENTED_EDGE('',*,*,#5485,.T.);
#7770=ORIENTED_EDGE('',*,*,#5348,.T.);
#7771=ORIENTED_EDGE('',*,*,#5326,.T.);
#7772=ORIENTED_EDGE('',*,*,#5305,.F.);
#7773=ORIENTED_EDGE('',*,*,#5488,.T.);
#7774=ORIENTED_EDGE('',*,*,#5492,.F.);
#7775=ORIENTED_EDGE('',*,*,#5493,.T.);
#7776=ORIENTED_EDGE('',*,*,#5318,.F.);
#7777=ORIENTED_EDGE('',*,*,#5493,.F.);
#7778=ORIENTED_EDGE('',*,*,#5494,.F.);
#7779=ORIENTED_EDGE('',*,*,#5490,.F.);
#7780=ORIENTED_EDGE('',*,*,#5387,.T.);
#7781=ORIENTED_EDGE('',*,*,#5467,.T.);
#7782=ORIENTED_EDGE('',*,*,#5398,.T.);
#7783=ORIENTED_EDGE('',*,*,#5394,.T.);
#7784=ORIENTED_EDGE('',*,*,#5466,.T.);
#7785=ORIENTED_EDGE('',*,*,#5419,.T.);
#7786=ORIENTED_EDGE('',*,*,#5415,.T.);
#7787=ORIENTED_EDGE('',*,*,#5495,.T.);
#7788=ORIENTED_EDGE('',*,*,#5491,.T.);
#7789=ORIENTED_EDGE('',*,*,#5496,.T.);
#7790=ORIENTED_EDGE('',*,*,#5468,.T.);
#7791=ORIENTED_EDGE('',*,*,#5391,.T.);
#7792=ORIENTED_EDGE('',*,*,#5495,.F.);
#7793=ORIENTED_EDGE('',*,*,#5418,.T.);
#7794=ORIENTED_EDGE('',*,*,#5446,.T.);
#7795=ORIENTED_EDGE('',*,*,#5481,.T.);
#7796=ORIENTED_EDGE('',*,*,#5474,.F.);
#7797=ORIENTED_EDGE('',*,*,#5441,.T.);
#7798=ORIENTED_EDGE('',*,*,#5497,.T.);
#7799=ORIENTED_EDGE('',*,*,#5487,.T.);
#7800=ORIENTED_EDGE('',*,*,#5358,.T.);
#7801=ORIENTED_EDGE('',*,*,#5498,.T.);
#7802=ORIENTED_EDGE('',*,*,#5431,.T.);
#7803=ORIENTED_EDGE('',*,*,#5435,.T.);
#7804=ORIENTED_EDGE('',*,*,#5462,.T.);
#7805=ORIENTED_EDGE('',*,*,#5499,.T.);
#7806=ORIENTED_EDGE('',*,*,#5492,.T.);
#7807=ORIENTED_EDGE('',*,*,#5497,.F.);
#7808=ORIENTED_EDGE('',*,*,#5440,.T.);
#7809=ORIENTED_EDGE('',*,*,#5436,.T.);
#7810=ORIENTED_EDGE('',*,*,#5459,.T.);
#7811=ORIENTED_EDGE('',*,*,#5354,.T.);
#7812=ORIENTED_EDGE('',*,*,#5365,.T.);
#7813=ORIENTED_EDGE('',*,*,#5473,.T.);
#7814=ORIENTED_EDGE('',*,*,#5424,.T.);
#7815=ORIENTED_EDGE('',*,*,#5428,.T.);
#7816=ORIENTED_EDGE('',*,*,#5464,.T.);
#7817=ORIENTED_EDGE('',*,*,#5368,.T.);
#7818=ORIENTED_EDGE('',*,*,#5372,.T.);
#7819=ORIENTED_EDGE('',*,*,#5472,.T.);
#7820=ORIENTED_EDGE('',*,*,#5375,.T.);
#7821=ORIENTED_EDGE('',*,*,#5379,.T.);
#7822=ORIENTED_EDGE('',*,*,#5471,.T.);
#7823=ORIENTED_EDGE('',*,*,#5410,.T.);
#7824=ORIENTED_EDGE('',*,*,#5414,.T.);
#7825=ORIENTED_EDGE('',*,*,#5465,.T.);
#7826=ORIENTED_EDGE('',*,*,#5382,.T.);
#7827=ORIENTED_EDGE('',*,*,#5386,.T.);
#7828=ORIENTED_EDGE('',*,*,#5470,.T.);
#7829=ORIENTED_EDGE('',*,*,#5403,.T.);
#7830=ORIENTED_EDGE('',*,*,#5407,.T.);
#7831=ORIENTED_EDGE('',*,*,#5469,.T.);
#7832=ORIENTED_EDGE('',*,*,#5496,.F.);
#7833=ORIENTED_EDGE('',*,*,#5494,.T.);
#7834=ORIENTED_EDGE('',*,*,#5499,.F.);
#7835=ORIENTED_EDGE('',*,*,#5461,.T.);
#7836=ORIENTED_EDGE('',*,*,#5361,.T.);
#7837=ORIENTED_EDGE('',*,*,#5357,.T.);
#7838=ORIENTED_EDGE('',*,*,#5476,.F.);
#7839=ORIENTED_EDGE('',*,*,#5432,.T.);
#7840=ORIENTED_EDGE('',*,*,#5498,.F.);
#7841=ORIENTED_EDGE('',*,*,#5320,.F.);
#7842=ORIENTED_EDGE('',*,*,#5500,.T.);
#7843=ORIENTED_EDGE('',*,*,#5475,.F.);
#7844=ORIENTED_EDGE('',*,*,#5486,.T.);
#7845=ORIENTED_EDGE('',*,*,#5325,.F.);
#7846=ORIENTED_EDGE('',*,*,#5489,.F.);
#7847=ORIENTED_EDGE('',*,*,#5451,.F.);
#7848=ORIENTED_EDGE('',*,*,#5500,.F.);
#7849=ORIENTED_EDGE('',*,*,#5478,.F.);
#7850=ORIENTED_EDGE('',*,*,#5346,.T.);
#7851=ORIENTED_EDGE('',*,*,#5343,.T.);
#7852=ORIENTED_EDGE('',*,*,#5484,.F.);
#7853=ORIENTED_EDGE('',*,*,#5350,.T.);
#7854=ORIENTED_EDGE('',*,*,#5351,.T.);
#7855=ORIENTED_EDGE('',*,*,#5501,.T.);
#7856=ORIENTED_EDGE('',*,*,#5502,.F.);
#7857=ORIENTED_EDGE('',*,*,#5501,.F.);
#7858=ORIENTED_EDGE('',*,*,#5338,.T.);
#7859=ORIENTED_EDGE('',*,*,#5339,.T.);
#7860=ORIENTED_EDGE('',*,*,#5503,.F.);
#7861=ORIENTED_EDGE('',*,*,#5502,.T.);
#7862=ORIENTED_EDGE('',*,*,#5345,.F.);
#7863=ORIENTED_EDGE('',*,*,#5504,.T.);
#7864=ORIENTED_EDGE('',*,*,#5503,.T.);
#7865=ORIENTED_EDGE('',*,*,#5504,.F.);
#7866=ORIENTED_EDGE('',*,*,#5505,.F.);
#7867=ORIENTED_EDGE('',*,*,#5506,.T.);
#7868=ORIENTED_EDGE('',*,*,#5507,.T.);
#7869=ORIENTED_EDGE('',*,*,#5508,.T.);
#7870=ORIENTED_EDGE('',*,*,#5509,.F.);
#7871=ORIENTED_EDGE('',*,*,#5510,.T.);
#7872=ORIENTED_EDGE('',*,*,#5505,.T.);
#7873=ORIENTED_EDGE('',*,*,#5511,.T.);
#7874=ORIENTED_EDGE('',*,*,#5512,.F.);
#7875=ORIENTED_EDGE('',*,*,#5513,.T.);
#7876=ORIENTED_EDGE('',*,*,#5509,.T.);
#7877=ORIENTED_EDGE('',*,*,#5514,.T.);
#7878=ORIENTED_EDGE('',*,*,#5515,.F.);
#7879=ORIENTED_EDGE('',*,*,#5516,.T.);
#7880=ORIENTED_EDGE('',*,*,#5512,.T.);
#7881=ORIENTED_EDGE('',*,*,#5517,.T.);
#7882=ORIENTED_EDGE('',*,*,#5518,.F.);
#7883=ORIENTED_EDGE('',*,*,#5519,.T.);
#7884=ORIENTED_EDGE('',*,*,#5515,.T.);
#7885=ORIENTED_EDGE('',*,*,#5520,.T.);
#7886=ORIENTED_EDGE('',*,*,#5521,.F.);
#7887=ORIENTED_EDGE('',*,*,#5522,.T.);
#7888=ORIENTED_EDGE('',*,*,#5523,.F.);
#7889=ORIENTED_EDGE('',*,*,#5524,.F.);
#7890=ORIENTED_EDGE('',*,*,#5525,.T.);
#7891=ORIENTED_EDGE('',*,*,#5521,.T.);
#7892=ORIENTED_EDGE('',*,*,#5526,.F.);
#7893=ORIENTED_EDGE('',*,*,#5527,.F.);
#7894=ORIENTED_EDGE('',*,*,#5528,.F.);
#7895=ORIENTED_EDGE('',*,*,#5529,.T.);
#7896=ORIENTED_EDGE('',*,*,#5524,.T.);
#7897=ORIENTED_EDGE('',*,*,#5530,.F.);
#7898=ORIENTED_EDGE('',*,*,#5531,.F.);
#7899=ORIENTED_EDGE('',*,*,#5532,.T.);
#7900=ORIENTED_EDGE('',*,*,#5528,.T.);
#7901=ORIENTED_EDGE('',*,*,#5533,.F.);
#7902=ORIENTED_EDGE('',*,*,#5534,.F.);
#7903=ORIENTED_EDGE('',*,*,#5535,.T.);
#7904=ORIENTED_EDGE('',*,*,#5531,.T.);
#7905=ORIENTED_EDGE('',*,*,#5536,.F.);
#7906=ORIENTED_EDGE('',*,*,#5526,.T.);
#7907=ORIENTED_EDGE('',*,*,#5523,.T.);
#7908=ORIENTED_EDGE('',*,*,#5537,.T.);
#7909=ORIENTED_EDGE('',*,*,#5538,.F.);
#7910=ORIENTED_EDGE('',*,*,#5539,.F.);
#7911=ORIENTED_EDGE('',*,*,#5540,.T.);
#7912=ORIENTED_EDGE('',*,*,#5540,.F.);
#7913=ORIENTED_EDGE('',*,*,#5541,.F.);
#7914=ORIENTED_EDGE('',*,*,#5520,.F.);
#7915=ORIENTED_EDGE('',*,*,#5517,.F.);
#7916=ORIENTED_EDGE('',*,*,#5514,.F.);
#7917=ORIENTED_EDGE('',*,*,#5511,.F.);
#7918=ORIENTED_EDGE('',*,*,#5508,.F.);
#7919=ORIENTED_EDGE('',*,*,#5542,.F.);
#7920=ORIENTED_EDGE('',*,*,#5543,.T.);
#7921=ORIENTED_EDGE('',*,*,#5536,.T.);
#7922=ORIENTED_EDGE('',*,*,#5533,.T.);
#7923=ORIENTED_EDGE('',*,*,#5530,.T.);
#7924=ORIENTED_EDGE('',*,*,#5527,.T.);
#7925=ORIENTED_EDGE('',*,*,#5544,.T.);
#7926=ORIENTED_EDGE('',*,*,#5545,.T.);
#7927=ORIENTED_EDGE('',*,*,#5546,.T.);
#7928=ORIENTED_EDGE('',*,*,#5547,.T.);
#7929=ORIENTED_EDGE('',*,*,#5542,.T.);
#7930=ORIENTED_EDGE('',*,*,#5534,.T.);
#7931=ORIENTED_EDGE('',*,*,#5543,.F.);
#7932=ORIENTED_EDGE('',*,*,#5547,.F.);
#7933=ORIENTED_EDGE('',*,*,#5548,.T.);
#7934=ORIENTED_EDGE('',*,*,#5537,.F.);
#7935=ORIENTED_EDGE('',*,*,#5522,.F.);
#7936=ORIENTED_EDGE('',*,*,#5525,.F.);
#7937=ORIENTED_EDGE('',*,*,#5529,.F.);
#7938=ORIENTED_EDGE('',*,*,#5532,.F.);
#7939=ORIENTED_EDGE('',*,*,#5535,.F.);
#7940=ORIENTED_EDGE('',*,*,#5548,.F.);
#7941=ORIENTED_EDGE('',*,*,#5546,.F.);
#7942=ORIENTED_EDGE('',*,*,#5506,.F.);
#7943=ORIENTED_EDGE('',*,*,#5510,.F.);
#7944=ORIENTED_EDGE('',*,*,#5513,.F.);
#7945=ORIENTED_EDGE('',*,*,#5516,.F.);
#7946=ORIENTED_EDGE('',*,*,#5519,.F.);
#7947=ORIENTED_EDGE('',*,*,#5549,.F.);
#7948=ORIENTED_EDGE('',*,*,#5550,.F.);
#7949=ORIENTED_EDGE('',*,*,#5551,.T.);
#7950=ORIENTED_EDGE('',*,*,#5552,.T.);
#7951=ORIENTED_EDGE('',*,*,#5553,.F.);
#7952=ORIENTED_EDGE('',*,*,#5554,.F.);
#7953=ORIENTED_EDGE('',*,*,#5555,.T.);
#7954=ORIENTED_EDGE('',*,*,#5556,.T.);
#7955=ORIENTED_EDGE('',*,*,#5551,.F.);
#7956=ORIENTED_EDGE('',*,*,#5557,.F.);
#7957=ORIENTED_EDGE('',*,*,#5558,.T.);
#7958=ORIENTED_EDGE('',*,*,#5559,.T.);
#7959=ORIENTED_EDGE('',*,*,#5555,.F.);
#7960=ORIENTED_EDGE('',*,*,#5560,.F.);
#7961=ORIENTED_EDGE('',*,*,#5561,.T.);
#7962=ORIENTED_EDGE('',*,*,#5562,.T.);
#7963=ORIENTED_EDGE('',*,*,#5558,.F.);
#7964=ORIENTED_EDGE('',*,*,#5563,.F.);
#7965=ORIENTED_EDGE('',*,*,#5564,.T.);
#7966=ORIENTED_EDGE('',*,*,#5565,.T.);
#7967=ORIENTED_EDGE('',*,*,#5561,.F.);
#7968=ORIENTED_EDGE('',*,*,#5566,.F.);
#7969=ORIENTED_EDGE('',*,*,#5553,.T.);
#7970=ORIENTED_EDGE('',*,*,#5567,.T.);
#7971=ORIENTED_EDGE('',*,*,#5564,.F.);
#7972=ORIENTED_EDGE('',*,*,#5567,.F.);
#7973=ORIENTED_EDGE('',*,*,#5552,.F.);
#7974=ORIENTED_EDGE('',*,*,#5556,.F.);
#7975=ORIENTED_EDGE('',*,*,#5559,.F.);
#7976=ORIENTED_EDGE('',*,*,#5562,.F.);
#7977=ORIENTED_EDGE('',*,*,#5565,.F.);
#7978=ORIENTED_EDGE('',*,*,#5568,.F.);
#7979=ORIENTED_EDGE('',*,*,#5544,.F.);
#7980=ORIENTED_EDGE('',*,*,#5507,.F.);
#7981=ORIENTED_EDGE('',*,*,#5545,.F.);
#7982=ORIENTED_EDGE('',*,*,#5569,.T.);
#7983=ORIENTED_EDGE('',*,*,#5568,.T.);
#7984=ORIENTED_EDGE('',*,*,#5569,.F.);
#7985=ORIENTED_EDGE('',*,*,#5518,.T.);
#7986=ORIENTED_EDGE('',*,*,#5541,.T.);
#7987=ORIENTED_EDGE('',*,*,#5570,.F.);
#7988=ORIENTED_EDGE('',*,*,#5549,.T.);
#7989=ORIENTED_EDGE('',*,*,#5571,.F.);
#7990=ORIENTED_EDGE('',*,*,#5572,.T.);
#7991=ORIENTED_EDGE('',*,*,#5538,.T.);
#7992=ORIENTED_EDGE('',*,*,#5570,.T.);
#7993=ORIENTED_EDGE('',*,*,#5539,.T.);
#7994=ORIENTED_EDGE('',*,*,#5572,.F.);
#7995=ORIENTED_EDGE('',*,*,#5571,.T.);
#7996=ORIENTED_EDGE('',*,*,#5550,.T.);
#7997=ORIENTED_EDGE('',*,*,#5566,.T.);
#7998=ORIENTED_EDGE('',*,*,#5563,.T.);
#7999=ORIENTED_EDGE('',*,*,#5560,.T.);
#8000=ORIENTED_EDGE('',*,*,#5557,.T.);
#8001=ORIENTED_EDGE('',*,*,#5554,.T.);
#8002=ORIENTED_EDGE('',*,*,#5573,.F.);
#8003=ORIENTED_EDGE('',*,*,#5574,.T.);
#8004=ORIENTED_EDGE('',*,*,#5575,.T.);
#8005=ORIENTED_EDGE('',*,*,#5576,.T.);
#8006=ORIENTED_EDGE('',*,*,#5577,.F.);
#8007=ORIENTED_EDGE('',*,*,#5578,.T.);
#8008=ORIENTED_EDGE('',*,*,#5573,.T.);
#8009=ORIENTED_EDGE('',*,*,#5579,.T.);
#8010=ORIENTED_EDGE('',*,*,#5580,.F.);
#8011=ORIENTED_EDGE('',*,*,#5581,.T.);
#8012=ORIENTED_EDGE('',*,*,#5577,.T.);
#8013=ORIENTED_EDGE('',*,*,#5582,.T.);
#8014=ORIENTED_EDGE('',*,*,#5583,.F.);
#8015=ORIENTED_EDGE('',*,*,#5584,.T.);
#8016=ORIENTED_EDGE('',*,*,#5580,.T.);
#8017=ORIENTED_EDGE('',*,*,#5585,.T.);
#8018=ORIENTED_EDGE('',*,*,#5586,.F.);
#8019=ORIENTED_EDGE('',*,*,#5587,.T.);
#8020=ORIENTED_EDGE('',*,*,#5583,.T.);
#8021=ORIENTED_EDGE('',*,*,#5588,.T.);
#8022=ORIENTED_EDGE('',*,*,#5589,.F.);
#8023=ORIENTED_EDGE('',*,*,#5590,.T.);
#8024=ORIENTED_EDGE('',*,*,#5586,.T.);
#8025=ORIENTED_EDGE('',*,*,#5591,.T.);
#8026=ORIENTED_EDGE('',*,*,#5592,.F.);
#8027=ORIENTED_EDGE('',*,*,#5593,.T.);
#8028=ORIENTED_EDGE('',*,*,#5589,.T.);
#8029=ORIENTED_EDGE('',*,*,#5594,.T.);
#8030=ORIENTED_EDGE('',*,*,#5595,.F.);
#8031=ORIENTED_EDGE('',*,*,#5596,.T.);
#8032=ORIENTED_EDGE('',*,*,#5592,.T.);
#8033=ORIENTED_EDGE('',*,*,#5597,.T.);
#8034=ORIENTED_EDGE('',*,*,#5598,.F.);
#8035=ORIENTED_EDGE('',*,*,#5599,.T.);
#8036=ORIENTED_EDGE('',*,*,#5595,.T.);
#8037=ORIENTED_EDGE('',*,*,#5600,.T.);
#8038=ORIENTED_EDGE('',*,*,#5601,.F.);
#8039=ORIENTED_EDGE('',*,*,#5602,.T.);
#8040=ORIENTED_EDGE('',*,*,#5598,.T.);
#8041=ORIENTED_EDGE('',*,*,#5603,.T.);
#8042=ORIENTED_EDGE('',*,*,#5604,.F.);
#8043=ORIENTED_EDGE('',*,*,#5605,.T.);
#8044=ORIENTED_EDGE('',*,*,#5601,.T.);
#8045=ORIENTED_EDGE('',*,*,#5606,.T.);
#8046=ORIENTED_EDGE('',*,*,#5607,.F.);
#8047=ORIENTED_EDGE('',*,*,#5608,.T.);
#8048=ORIENTED_EDGE('',*,*,#5604,.T.);
#8049=ORIENTED_EDGE('',*,*,#5609,.T.);
#8050=ORIENTED_EDGE('',*,*,#5610,.F.);
#8051=ORIENTED_EDGE('',*,*,#5611,.T.);
#8052=ORIENTED_EDGE('',*,*,#5612,.F.);
#8053=ORIENTED_EDGE('',*,*,#5613,.F.);
#8054=ORIENTED_EDGE('',*,*,#5614,.F.);
#8055=ORIENTED_EDGE('',*,*,#5615,.T.);
#8056=ORIENTED_EDGE('',*,*,#5610,.T.);
#8057=ORIENTED_EDGE('',*,*,#5616,.F.);
#8058=ORIENTED_EDGE('',*,*,#5617,.F.);
#8059=ORIENTED_EDGE('',*,*,#5618,.T.);
#8060=ORIENTED_EDGE('',*,*,#5614,.T.);
#8061=ORIENTED_EDGE('',*,*,#5619,.F.);
#8062=ORIENTED_EDGE('',*,*,#5620,.F.);
#8063=ORIENTED_EDGE('',*,*,#5621,.T.);
#8064=ORIENTED_EDGE('',*,*,#5617,.T.);
#8065=ORIENTED_EDGE('',*,*,#5622,.F.);
#8066=ORIENTED_EDGE('',*,*,#5623,.F.);
#8067=ORIENTED_EDGE('',*,*,#5624,.T.);
#8068=ORIENTED_EDGE('',*,*,#5620,.T.);
#8069=ORIENTED_EDGE('',*,*,#5625,.F.);
#8070=ORIENTED_EDGE('',*,*,#5626,.F.);
#8071=ORIENTED_EDGE('',*,*,#5627,.T.);
#8072=ORIENTED_EDGE('',*,*,#5623,.T.);
#8073=ORIENTED_EDGE('',*,*,#5628,.F.);
#8074=ORIENTED_EDGE('',*,*,#5629,.F.);
#8075=ORIENTED_EDGE('',*,*,#5630,.T.);
#8076=ORIENTED_EDGE('',*,*,#5626,.T.);
#8077=ORIENTED_EDGE('',*,*,#5631,.F.);
#8078=ORIENTED_EDGE('',*,*,#5632,.F.);
#8079=ORIENTED_EDGE('',*,*,#5633,.T.);
#8080=ORIENTED_EDGE('',*,*,#5629,.T.);
#8081=ORIENTED_EDGE('',*,*,#5634,.F.);
#8082=ORIENTED_EDGE('',*,*,#5635,.F.);
#8083=ORIENTED_EDGE('',*,*,#5636,.T.);
#8084=ORIENTED_EDGE('',*,*,#5632,.T.);
#8085=ORIENTED_EDGE('',*,*,#5637,.F.);
#8086=ORIENTED_EDGE('',*,*,#5638,.F.);
#8087=ORIENTED_EDGE('',*,*,#5639,.T.);
#8088=ORIENTED_EDGE('',*,*,#5635,.T.);
#8089=ORIENTED_EDGE('',*,*,#5640,.F.);
#8090=ORIENTED_EDGE('',*,*,#5641,.F.);
#8091=ORIENTED_EDGE('',*,*,#5642,.T.);
#8092=ORIENTED_EDGE('',*,*,#5638,.T.);
#8093=ORIENTED_EDGE('',*,*,#5643,.F.);
#8094=ORIENTED_EDGE('',*,*,#5644,.F.);
#8095=ORIENTED_EDGE('',*,*,#5645,.T.);
#8096=ORIENTED_EDGE('',*,*,#5641,.T.);
#8097=ORIENTED_EDGE('',*,*,#5646,.F.);
#8098=ORIENTED_EDGE('',*,*,#5612,.T.);
#8099=ORIENTED_EDGE('',*,*,#5647,.T.);
#8100=ORIENTED_EDGE('',*,*,#5648,.F.);
#8101=ORIENTED_EDGE('',*,*,#5649,.F.);
#8102=ORIENTED_EDGE('',*,*,#5650,.T.);
#8103=ORIENTED_EDGE('',*,*,#5650,.F.);
#8104=ORIENTED_EDGE('',*,*,#5651,.F.);
#8105=ORIENTED_EDGE('',*,*,#5609,.F.);
#8106=ORIENTED_EDGE('',*,*,#5606,.F.);
#8107=ORIENTED_EDGE('',*,*,#5603,.F.);
#8108=ORIENTED_EDGE('',*,*,#5600,.F.);
#8109=ORIENTED_EDGE('',*,*,#5597,.F.);
#8110=ORIENTED_EDGE('',*,*,#5594,.F.);
#8111=ORIENTED_EDGE('',*,*,#5591,.F.);
#8112=ORIENTED_EDGE('',*,*,#5588,.F.);
#8113=ORIENTED_EDGE('',*,*,#5585,.F.);
#8114=ORIENTED_EDGE('',*,*,#5582,.F.);
#8115=ORIENTED_EDGE('',*,*,#5579,.F.);
#8116=ORIENTED_EDGE('',*,*,#5576,.F.);
#8117=ORIENTED_EDGE('',*,*,#5652,.F.);
#8118=ORIENTED_EDGE('',*,*,#5653,.T.);
#8119=ORIENTED_EDGE('',*,*,#5646,.T.);
#8120=ORIENTED_EDGE('',*,*,#5643,.T.);
#8121=ORIENTED_EDGE('',*,*,#5640,.T.);
#8122=ORIENTED_EDGE('',*,*,#5637,.T.);
#8123=ORIENTED_EDGE('',*,*,#5634,.T.);
#8124=ORIENTED_EDGE('',*,*,#5631,.T.);
#8125=ORIENTED_EDGE('',*,*,#5628,.T.);
#8126=ORIENTED_EDGE('',*,*,#5625,.T.);
#8127=ORIENTED_EDGE('',*,*,#5622,.T.);
#8128=ORIENTED_EDGE('',*,*,#5619,.T.);
#8129=ORIENTED_EDGE('',*,*,#5616,.T.);
#8130=ORIENTED_EDGE('',*,*,#5613,.T.);
#8131=ORIENTED_EDGE('',*,*,#5654,.T.);
#8132=ORIENTED_EDGE('',*,*,#5655,.T.);
#8133=ORIENTED_EDGE('',*,*,#5656,.T.);
#8134=ORIENTED_EDGE('',*,*,#5657,.T.);
#8135=ORIENTED_EDGE('',*,*,#5652,.T.);
#8136=ORIENTED_EDGE('',*,*,#5644,.T.);
#8137=ORIENTED_EDGE('',*,*,#5653,.F.);
#8138=ORIENTED_EDGE('',*,*,#5657,.F.);
#8139=ORIENTED_EDGE('',*,*,#5658,.T.);
#8140=ORIENTED_EDGE('',*,*,#5647,.F.);
#8141=ORIENTED_EDGE('',*,*,#5611,.F.);
#8142=ORIENTED_EDGE('',*,*,#5615,.F.);
#8143=ORIENTED_EDGE('',*,*,#5618,.F.);
#8144=ORIENTED_EDGE('',*,*,#5621,.F.);
#8145=ORIENTED_EDGE('',*,*,#5624,.F.);
#8146=ORIENTED_EDGE('',*,*,#5627,.F.);
#8147=ORIENTED_EDGE('',*,*,#5630,.F.);
#8148=ORIENTED_EDGE('',*,*,#5633,.F.);
#8149=ORIENTED_EDGE('',*,*,#5636,.F.);
#8150=ORIENTED_EDGE('',*,*,#5639,.F.);
#8151=ORIENTED_EDGE('',*,*,#5642,.F.);
#8152=ORIENTED_EDGE('',*,*,#5645,.F.);
#8153=ORIENTED_EDGE('',*,*,#5658,.F.);
#8154=ORIENTED_EDGE('',*,*,#5656,.F.);
#8155=ORIENTED_EDGE('',*,*,#5574,.F.);
#8156=ORIENTED_EDGE('',*,*,#5578,.F.);
#8157=ORIENTED_EDGE('',*,*,#5581,.F.);
#8158=ORIENTED_EDGE('',*,*,#5584,.F.);
#8159=ORIENTED_EDGE('',*,*,#5587,.F.);
#8160=ORIENTED_EDGE('',*,*,#5590,.F.);
#8161=ORIENTED_EDGE('',*,*,#5593,.F.);
#8162=ORIENTED_EDGE('',*,*,#5596,.F.);
#8163=ORIENTED_EDGE('',*,*,#5599,.F.);
#8164=ORIENTED_EDGE('',*,*,#5602,.F.);
#8165=ORIENTED_EDGE('',*,*,#5605,.F.);
#8166=ORIENTED_EDGE('',*,*,#5608,.F.);
#8167=ORIENTED_EDGE('',*,*,#5659,.F.);
#8168=ORIENTED_EDGE('',*,*,#5660,.T.);
#8169=ORIENTED_EDGE('',*,*,#5661,.F.);
#8170=ORIENTED_EDGE('',*,*,#5660,.F.);
#8171=ORIENTED_EDGE('',*,*,#5662,.F.);
#8172=ORIENTED_EDGE('',*,*,#5663,.T.);
#8173=ORIENTED_EDGE('',*,*,#5664,.T.);
#8174=ORIENTED_EDGE('',*,*,#5665,.F.);
#8175=ORIENTED_EDGE('',*,*,#5666,.F.);
#8176=ORIENTED_EDGE('',*,*,#5667,.T.);
#8177=ORIENTED_EDGE('',*,*,#5668,.T.);
#8178=ORIENTED_EDGE('',*,*,#5663,.F.);
#8179=ORIENTED_EDGE('',*,*,#5669,.F.);
#8180=ORIENTED_EDGE('',*,*,#5670,.T.);
#8181=ORIENTED_EDGE('',*,*,#5671,.T.);
#8182=ORIENTED_EDGE('',*,*,#5667,.F.);
#8183=ORIENTED_EDGE('',*,*,#5672,.F.);
#8184=ORIENTED_EDGE('',*,*,#5673,.T.);
#8185=ORIENTED_EDGE('',*,*,#5674,.T.);
#8186=ORIENTED_EDGE('',*,*,#5670,.F.);
#8187=ORIENTED_EDGE('',*,*,#5675,.F.);
#8188=ORIENTED_EDGE('',*,*,#5676,.T.);
#8189=ORIENTED_EDGE('',*,*,#5677,.T.);
#8190=ORIENTED_EDGE('',*,*,#5673,.F.);
#8191=ORIENTED_EDGE('',*,*,#5678,.F.);
#8192=ORIENTED_EDGE('',*,*,#5665,.T.);
#8193=ORIENTED_EDGE('',*,*,#5679,.T.);
#8194=ORIENTED_EDGE('',*,*,#5676,.F.);
#8195=ORIENTED_EDGE('',*,*,#5679,.F.);
#8196=ORIENTED_EDGE('',*,*,#5664,.F.);
#8197=ORIENTED_EDGE('',*,*,#5668,.F.);
#8198=ORIENTED_EDGE('',*,*,#5671,.F.);
#8199=ORIENTED_EDGE('',*,*,#5674,.F.);
#8200=ORIENTED_EDGE('',*,*,#5677,.F.);
#8201=ORIENTED_EDGE('',*,*,#5661,.T.);
#8202=ORIENTED_EDGE('',*,*,#5680,.F.);
#8203=ORIENTED_EDGE('',*,*,#5654,.F.);
#8204=ORIENTED_EDGE('',*,*,#5575,.F.);
#8205=ORIENTED_EDGE('',*,*,#5655,.F.);
#8206=ORIENTED_EDGE('',*,*,#5681,.T.);
#8207=ORIENTED_EDGE('',*,*,#5680,.T.);
#8208=ORIENTED_EDGE('',*,*,#5681,.F.);
#8209=ORIENTED_EDGE('',*,*,#5607,.T.);
#8210=ORIENTED_EDGE('',*,*,#5651,.T.);
#8211=ORIENTED_EDGE('',*,*,#5682,.F.);
#8212=ORIENTED_EDGE('',*,*,#5659,.T.);
#8213=ORIENTED_EDGE('',*,*,#5683,.F.);
#8214=ORIENTED_EDGE('',*,*,#5684,.T.);
#8215=ORIENTED_EDGE('',*,*,#5648,.T.);
#8216=ORIENTED_EDGE('',*,*,#5682,.T.);
#8217=ORIENTED_EDGE('',*,*,#5649,.T.);
#8218=ORIENTED_EDGE('',*,*,#5684,.F.);
#8219=ORIENTED_EDGE('',*,*,#5683,.T.);
#8220=ORIENTED_EDGE('',*,*,#5662,.T.);
#8221=ORIENTED_EDGE('',*,*,#5678,.T.);
#8222=ORIENTED_EDGE('',*,*,#5675,.T.);
#8223=ORIENTED_EDGE('',*,*,#5672,.T.);
#8224=ORIENTED_EDGE('',*,*,#5669,.T.);
#8225=ORIENTED_EDGE('',*,*,#5666,.T.);
#8226=ORIENTED_EDGE('',*,*,#5685,.F.);
#8227=ORIENTED_EDGE('',*,*,#5686,.F.);
#8228=ORIENTED_EDGE('',*,*,#5687,.T.);
#8229=ORIENTED_EDGE('',*,*,#5685,.T.);
#8230=ORIENTED_EDGE('',*,*,#5687,.F.);
#8231=ORIENTED_EDGE('',*,*,#5688,.F.);
#8232=ORIENTED_EDGE('',*,*,#5689,.T.);
#8233=ORIENTED_EDGE('',*,*,#5686,.T.);
#8234=ORIENTED_EDGE('',*,*,#5689,.F.);
#8235=ORIENTED_EDGE('',*,*,#5690,.F.);
#8236=ORIENTED_EDGE('',*,*,#5691,.T.);
#8237=ORIENTED_EDGE('',*,*,#5688,.T.);
#8238=ORIENTED_EDGE('',*,*,#5691,.F.);
#8239=ORIENTED_EDGE('',*,*,#5690,.T.);
#8240=PLANE('',#9244);
#8241=PLANE('',#9245);
#8242=PLANE('',#9246);
#8243=PLANE('',#9247);
#8244=PLANE('',#9248);
#8245=PLANE('',#9250);
#8246=PLANE('',#9251);
#8247=PLANE('',#9252);
#8248=PLANE('',#9253);
#8249=PLANE('',#9255);
#8250=PLANE('',#9257);
#8251=PLANE('',#9258);
#8252=PLANE('',#9260);
#8253=PLANE('',#9264);
#8254=PLANE('',#9266);
#8255=PLANE('',#9275);
#8256=PLANE('',#9276);
#8257=PLANE('',#9278);
#8258=PLANE('',#9279);
#8259=PLANE('',#9280);
#8260=PLANE('',#9282);
#8261=PLANE('',#9283);
#8262=PLANE('',#9284);
#8263=PLANE('',#9285);
#8264=PLANE('',#9287);
#8265=PLANE('',#9288);
#8266=PLANE('',#9289);
#8267=PLANE('',#9290);
#8268=PLANE('',#9292);
#8269=PLANE('',#9294);
#8270=PLANE('',#9295);
#8271=PLANE('',#9297);
#8272=PLANE('',#9300);
#8273=PLANE('',#9301);
#8274=PLANE('',#9303);
#8275=PLANE('',#9307);
#8276=PLANE('',#9311);
#8277=PLANE('',#9315);
#8278=PLANE('',#9321);
#8279=PLANE('',#9324);
#8280=PLANE('',#9325);
#8281=PLANE('',#9331);
#8282=PLANE('',#9334);
#8283=PLANE('',#9337);
#8284=PLANE('',#9341);
#8285=PLANE('',#9345);
#8286=PLANE('',#9348);
#8287=PLANE('',#9351);
#8288=PLANE('',#9352);
#8289=PLANE('',#9353);
#8290=PLANE('',#9360);
#8291=PLANE('',#9368);
#8292=PLANE('',#9374);
#8293=PLANE('',#9375);
#8294=PLANE('',#9384);
#8295=PLANE('',#9385);
#8296=PLANE('',#9386);
#8297=PLANE('',#9387);
#8298=PLANE('',#9389);
#8299=PLANE('',#9392);
#8300=PLANE('',#9394);
#8301=PLANE('',#9396);
#8302=PLANE('',#9397);
#8303=PLANE('',#9398);
#8304=PLANE('',#9399);
#8305=PLANE('',#9400);
#8306=PLANE('',#9401);
#8307=PLANE('',#9402);
#8308=PLANE('',#9403);
#8309=PLANE('',#9404);
#8310=PLANE('',#9405);
#8311=PLANE('',#9406);
#8312=PLANE('',#9407);
#8313=PLANE('',#9408);
#8314=PLANE('',#9409);
#8315=PLANE('',#9410);
#8316=PLANE('',#9411);
#8317=PLANE('',#9412);
#8318=PLANE('',#9413);
#8319=PLANE('',#9414);
#8320=PLANE('',#9415);
#8321=PLANE('',#9416);
#8322=PLANE('',#9417);
#8323=PLANE('',#9418);
#8324=PLANE('',#9419);
#8325=PLANE('',#9420);
#8326=PLANE('',#9421);
#8327=PLANE('',#9422);
#8328=PLANE('',#9423);
#8329=PLANE('',#9424);
#8330=PLANE('',#9425);
#8331=PLANE('',#9426);
#8332=PLANE('',#9427);
#8333=PLANE('',#9428);
#8334=PLANE('',#9429);
#8335=PLANE('',#9430);
#8336=PLANE('',#9431);
#8337=PLANE('',#9432);
#8338=PLANE('',#9433);
#8339=PLANE('',#9434);
#8340=PLANE('',#9435);
#8341=PLANE('',#9436);
#8342=PLANE('',#9437);
#8343=PLANE('',#9438);
#8344=PLANE('',#9439);
#8345=PLANE('',#9440);
#8346=PLANE('',#9441);
#8347=PLANE('',#9442);
#8348=PLANE('',#9443);
#8349=PLANE('',#9444);
#8350=PLANE('',#9445);
#8351=PLANE('',#9446);
#8352=PLANE('',#9447);
#8353=PLANE('',#9448);
#8354=PLANE('',#9449);
#8355=PLANE('',#9450);
#8356=PLANE('',#9451);
#8357=PLANE('',#9452);
#8358=PLANE('',#9453);
#8359=PLANE('',#9454);
#8360=PLANE('',#9455);
#8361=PLANE('',#9456);
#8362=PLANE('',#9457);
#8363=PLANE('',#9458);
#8364=PLANE('',#9459);
#8365=PLANE('',#9460);
#8366=PLANE('',#9461);
#8367=PLANE('',#9469);
#8368=PLANE('',#9471);
#8369=PLANE('',#9475);
#8370=PLANE('',#9479);
#8371=PLANE('',#9483);
#8372=PLANE('',#9489);
#8373=PLANE('',#9492);
#8374=PLANE('',#9493);
#8375=PLANE('',#9502);
#8376=PLANE('',#9513);
#8377=PLANE('',#9516);
#8378=PLANE('',#9518);
#8379=PLANE('',#9520);
#8380=PLANE('',#9523);
#8381=PLANE('',#9525);
#8382=PLANE('',#9548);
#8383=PLANE('',#9557);
#8384=PLANE('',#9558);
#8385=PLANE('',#9559);
#8386=PLANE('',#9560);
#8387=PLANE('',#9561);
#8388=PLANE('',#9562);
#8389=PLANE('',#9563);
#8390=PLANE('',#9567);
#8391=PLANE('',#9576);
#8392=PLANE('',#9577);
#8393=PLANE('',#9578);
#8394=PLANE('',#9580);
#8395=PLANE('',#9581);
#8396=PLANE('',#9582);
#8397=PLANE('',#9584);
#8398=PLANE('',#9585);
#8399=PLANE('',#9586);
#8400=PLANE('',#9587);
#8401=PLANE('',#9588);
#8402=PLANE('',#9589);
#8403=PLANE('',#9590);
#8404=PLANE('',#9592);
#8405=PLANE('',#9594);
#8406=PLANE('',#9599);
#8407=PLANE('',#9600);
#8408=PLANE('',#9601);
#8409=PLANE('',#9602);
#8410=PLANE('',#9603);
#8411=PLANE('',#9604);
#8412=PLANE('',#9605);
#8413=PLANE('',#9606);
#8414=PLANE('',#9607);
#8415=PLANE('',#9608);
#8416=PLANE('',#9609);
#8417=PLANE('',#9610);
#8418=PLANE('',#9611);
#8419=PLANE('',#9612);
#8420=PLANE('',#9613);
#8421=PLANE('',#9614);
#8422=PLANE('',#9615);
#8423=PLANE('',#9616);
#8424=PLANE('',#9617);
#8425=PLANE('',#9618);
#8426=PLANE('',#9619);
#8427=PLANE('',#9620);
#8428=PLANE('',#9621);
#8429=PLANE('',#9622);
#8430=PLANE('',#9623);
#8431=PLANE('',#9624);
#8432=PLANE('',#9625);
#8433=PLANE('',#9626);
#8434=PLANE('',#9627);
#8435=PLANE('',#9628);
#8436=PLANE('',#9629);
#8437=PLANE('',#9630);
#8438=PLANE('',#9631);
#8439=PLANE('',#9632);
#8440=PLANE('',#9633);
#8441=PLANE('',#9634);
#8442=PLANE('',#9635);
#8443=PLANE('',#9636);
#8444=PLANE('',#9637);
#8445=PLANE('',#9638);
#8446=PLANE('',#9639);
#8447=PLANE('',#9640);
#8448=PLANE('',#9641);
#8449=PLANE('',#9642);
#8450=PLANE('',#9643);
#8451=PLANE('',#9644);
#8452=PLANE('',#9648);
#8453=PLANE('',#9649);
#8454=PLANE('',#9650);
#8455=PLANE('',#9651);
#8456=PLANE('',#9652);
#8457=PLANE('',#9653);
#8458=PLANE('',#9654);
#8459=PLANE('',#9655);
#8460=PLANE('',#9656);
#8461=PLANE('',#9657);
#8462=PLANE('',#9658);
#8463=PLANE('',#9659);
#8464=PLANE('',#9663);
#8465=PLANE('',#9665);
#8466=PLANE('',#9673);
#8467=PLANE('',#9681);
#8468=PLANE('',#9682);
#8469=PLANE('',#9687);
#8470=PLANE('',#9688);
#8471=PLANE('',#9690);
#8472=PLANE('',#9693);
#8473=PLANE('',#9701);
#8474=PLANE('',#9706);
#8475=PLANE('',#9712);
#8476=PLANE('',#9718);
#8477=PLANE('',#9724);
#8478=PLANE('',#9728);
#8479=PLANE('',#9733);
#8480=PLANE('',#9735);
#8481=PLANE('',#9740);
#8482=PLANE('',#9744);
#8483=PLANE('',#9745);
#8484=PLANE('',#9750);
#8485=PLANE('',#9764);
#8486=PLANE('',#9766);
#8487=PLANE('',#9767);
#8488=PLANE('',#9768);
#8489=PLANE('',#9769);
#8490=PLANE('',#9770);
#8491=PLANE('',#9771);
#8492=PLANE('',#9772);
#8493=PLANE('',#9773);
#8494=PLANE('',#9774);
#8495=PLANE('',#9775);
#8496=PLANE('',#9776);
#8497=PLANE('',#9777);
#8498=PLANE('',#9778);
#8499=PLANE('',#9779);
#8500=PLANE('',#9780);
#8501=PLANE('',#9781);
#8502=PLANE('',#9782);
#8503=PLANE('',#9783);
#8504=PLANE('',#9784);
#8505=PLANE('',#9785);
#8506=PLANE('',#9786);
#8507=PLANE('',#9787);
#8508=PLANE('',#9788);
#8509=PLANE('',#9789);
#8510=PLANE('',#9790);
#8511=PLANE('',#9791);
#8512=PLANE('',#9797);
#8513=PLANE('',#9798);
#8514=PLANE('',#9801);
#8515=PLANE('',#9804);
#8516=PLANE('',#9805);
#8517=PLANE('',#9806);
#8518=PLANE('',#9808);
#8519=PLANE('',#9810);
#8520=PLANE('',#9812);
#8521=PLANE('',#9813);
#8522=PLANE('',#9814);
#8523=PLANE('',#9815);
#8524=PLANE('',#9819);
#8525=PLANE('',#9820);
#8526=PLANE('',#9821);
#8527=PLANE('',#9822);
#8528=PLANE('',#9824);
#8529=PLANE('',#9827);
#8530=PLANE('',#9830);
#8531=PLANE('',#9832);
#8532=PLANE('',#9833);
#8533=PLANE('',#9836);
#8534=PLANE('',#9837);
#8535=PLANE('',#9839);
#8536=PLANE('',#9840);
#8537=PLANE('',#9841);
#8538=PLANE('',#9844);
#8539=PLANE('',#9861);
#8540=PLANE('',#9864);
#8541=PLANE('',#9869);
#8542=PLANE('',#9870);
#8543=PLANE('',#9871);
#8544=PLANE('',#9872);
#8545=PLANE('',#9873);
#8546=PLANE('',#9874);
#8547=PLANE('',#9875);
#8548=PLANE('',#9876);
#8549=PLANE('',#9883);
#8550=PLANE('',#9911);
#8551=PLANE('',#9914);
#8552=PLANE('',#9921);
#8553=PLANE('',#9922);
#8554=PLANE('',#9923);
#8555=PLANE('',#9924);
#8556=PLANE('',#9925);
#8557=PLANE('',#9926);
#8558=PLANE('',#9927);
#8559=PLANE('',#9928);
#8560=PLANE('',#9935);
#8561=PLANE('',#9937);
#8562=PLANE('',#9945);
#8563=ADVANCED_FACE('',(#842),#8240,.T.);
#8564=ADVANCED_FACE('',(#843),#8241,.T.);
#8565=ADVANCED_FACE('',(#844),#8242,.T.);
#8566=ADVANCED_FACE('',(#845),#8243,.T.);
#8567=ADVANCED_FACE('',(#846),#8244,.T.);
#8568=ADVANCED_FACE('',(#847),#8245,.T.);
#8569=ADVANCED_FACE('',(#848),#8246,.T.);
#8570=ADVANCED_FACE('',(#849),#8247,.T.);
#8571=ADVANCED_FACE('',(#850),#8248,.T.);
#8572=ADVANCED_FACE('',(#851),#8249,.T.);
#8573=ADVANCED_FACE('',(#852),#8250,.T.);
#8574=ADVANCED_FACE('',(#853),#8251,.T.);
#8575=ADVANCED_FACE('',(#854,#579,#580,#581),#8252,.T.);
#8576=ADVANCED_FACE('',(#855),#8253,.T.);
#8577=ADVANCED_FACE('',(#856),#8254,.T.);
#8578=ADVANCED_FACE('',(#857),#494,.F.);
#8579=ADVANCED_FACE('',(#858),#495,.F.);
#8580=ADVANCED_FACE('',(#859),#496,.F.);
#8581=ADVANCED_FACE('',(#860),#497,.F.);
#8582=ADVANCED_FACE('',(#861),#8255,.F.);
#8583=ADVANCED_FACE('',(#862,#582,#583,#584),#8256,.T.);
#8584=ADVANCED_FACE('',(#863),#8257,.T.);
#8585=ADVANCED_FACE('',(#864),#8258,.T.);
#8586=ADVANCED_FACE('',(#865),#8259,.T.);
#8587=ADVANCED_FACE('',(#866),#8260,.T.);
#8588=ADVANCED_FACE('',(#867),#8261,.T.);
#8589=ADVANCED_FACE('',(#868),#8262,.T.);
#8590=ADVANCED_FACE('',(#869),#8263,.T.);
#8591=ADVANCED_FACE('',(#870),#8264,.T.);
#8592=ADVANCED_FACE('',(#871),#8265,.T.);
#8593=ADVANCED_FACE('',(#872),#8266,.T.);
#8594=ADVANCED_FACE('',(#873),#8267,.T.);
#8595=ADVANCED_FACE('',(#874),#8268,.T.);
#8596=ADVANCED_FACE('',(#875),#8269,.T.);
#8597=ADVANCED_FACE('',(#876),#8270,.T.);
#8598=ADVANCED_FACE('',(#877),#8271,.T.);
#8599=ADVANCED_FACE('',(#878),#498,.F.);
#8600=ADVANCED_FACE('',(#879),#8272,.F.);
#8601=ADVANCED_FACE('',(#880),#8273,.T.);
#8602=ADVANCED_FACE('',(#881),#8274,.T.);
#8603=ADVANCED_FACE('',(#882),#368,.T.);
#8604=ADVANCED_FACE('',(#883),#8275,.T.);
#8605=ADVANCED_FACE('',(#884),#369,.T.);
#8606=ADVANCED_FACE('',(#885),#8276,.T.);
#8607=ADVANCED_FACE('',(#886),#370,.T.);
#8608=ADVANCED_FACE('',(#887),#8277,.T.);
#8609=ADVANCED_FACE('',(#888),#371,.T.);
#8610=ADVANCED_FACE('',(#889),#499,.T.);
#8611=ADVANCED_FACE('',(#890),#8278,.T.);
#8612=ADVANCED_FACE('',(#891),#500,.T.);
#8613=ADVANCED_FACE('',(#892),#8279,.T.);
#8614=ADVANCED_FACE('',(#893,#585,#586,#587,#588,#589),#8280,.T.);
#8615=ADVANCED_FACE('',(#894),#8281,.T.);
#8616=ADVANCED_FACE('',(#895),#372,.T.);
#8617=ADVANCED_FACE('',(#896),#8282,.T.);
#8618=ADVANCED_FACE('',(#897),#373,.T.);
#8619=ADVANCED_FACE('',(#898),#8283,.T.);
#8620=ADVANCED_FACE('',(#899),#374,.T.);
#8621=ADVANCED_FACE('',(#900),#8284,.T.);
#8622=ADVANCED_FACE('',(#901),#375,.T.);
#8623=ADVANCED_FACE('',(#902),#8285,.T.);
#8624=ADVANCED_FACE('',(#903),#376,.T.);
#8625=ADVANCED_FACE('',(#904),#8286,.T.);
#8626=ADVANCED_FACE('',(#905),#377,.T.);
#8627=ADVANCED_FACE('',(#906),#8287,.T.);
#8628=ADVANCED_FACE('',(#907),#8288,.T.);
#8629=ADVANCED_FACE('',(#908),#143,.F.);
#8630=ADVANCED_FACE('',(#909),#8289,.T.);
#8631=ADVANCED_FACE('',(#910),#378,.F.);
#8632=ADVANCED_FACE('',(#911),#379,.T.);
#8633=ADVANCED_FACE('',(#912),#8290,.T.);
#8634=ADVANCED_FACE('',(#913),#380,.F.);
#8635=ADVANCED_FACE('',(#914),#381,.F.);
#8636=ADVANCED_FACE('',(#915),#382,.T.);
#8637=ADVANCED_FACE('',(#916),#8291,.T.);
#8638=ADVANCED_FACE('',(#917),#383,.F.);
#8639=ADVANCED_FACE('',(#918),#384,.F.);
#8640=ADVANCED_FACE('',(#919),#8292,.T.);
#8641=ADVANCED_FACE('',(#920,#590,#591,#592,#593,#594,#595,#596,#597),#8293,
 .T.);
#8642=ADVANCED_FACE('',(#921),#385,.F.);
#8643=ADVANCED_FACE('',(#922),#386,.F.);
#8644=ADVANCED_FACE('',(#923),#387,.F.);
#8645=ADVANCED_FACE('',(#924),#8294,.T.);
#8646=ADVANCED_FACE('',(#925),#8295,.F.);
#8647=ADVANCED_FACE('',(#926),#8296,.F.);
#8648=ADVANCED_FACE('',(#927),#8297,.T.);
#8649=ADVANCED_FACE('',(#928),#388,.T.);
#8650=ADVANCED_FACE('',(#929),#8298,.T.);
#8651=ADVANCED_FACE('',(#930),#389,.T.);
#8652=ADVANCED_FACE('',(#931),#8299,.T.);
#8653=ADVANCED_FACE('',(#932),#390,.T.);
#8654=ADVANCED_FACE('',(#933),#8300,.T.);
#8655=ADVANCED_FACE('',(#934),#391,.T.);
#8656=ADVANCED_FACE('',(#935),#8301,.F.);
#8657=ADVANCED_FACE('',(#936),#8302,.F.);
#8658=ADVANCED_FACE('',(#937),#8303,.T.);
#8659=ADVANCED_FACE('',(#938),#8304,.F.);
#8660=ADVANCED_FACE('',(#939),#8305,.F.);
#8661=ADVANCED_FACE('',(#940),#8306,.F.);
#8662=ADVANCED_FACE('',(#941),#8307,.F.);
#8663=ADVANCED_FACE('',(#942),#8308,.F.);
#8664=ADVANCED_FACE('',(#943),#8309,.F.);
#8665=ADVANCED_FACE('',(#944),#8310,.F.);
#8666=ADVANCED_FACE('',(#945),#8311,.F.);
#8667=ADVANCED_FACE('',(#946),#8312,.F.);
#8668=ADVANCED_FACE('',(#947),#8313,.F.);
#8669=ADVANCED_FACE('',(#948),#8314,.F.);
#8670=ADVANCED_FACE('',(#949),#8315,.F.);
#8671=ADVANCED_FACE('',(#950),#8316,.F.);
#8672=ADVANCED_FACE('',(#951),#8317,.F.);
#8673=ADVANCED_FACE('',(#952),#8318,.F.);
#8674=ADVANCED_FACE('',(#953),#8319,.F.);
#8675=ADVANCED_FACE('',(#954),#144,.F.);
#8676=ADVANCED_FACE('',(#955),#145,.F.);
#8677=ADVANCED_FACE('',(#956),#146,.F.);
#8678=ADVANCED_FACE('',(#957),#147,.F.);
#8679=ADVANCED_FACE('',(#958),#148,.F.);
#8680=ADVANCED_FACE('',(#959),#149,.F.);
#8681=ADVANCED_FACE('',(#960),#8320,.F.);
#8682=ADVANCED_FACE('',(#961),#8321,.F.);
#8683=ADVANCED_FACE('',(#962),#8322,.F.);
#8684=ADVANCED_FACE('',(#963),#8323,.F.);
#8685=ADVANCED_FACE('',(#964),#8324,.F.);
#8686=ADVANCED_FACE('',(#965),#8325,.F.);
#8687=ADVANCED_FACE('',(#966),#8326,.F.);
#8688=ADVANCED_FACE('',(#967),#8327,.F.);
#8689=ADVANCED_FACE('',(#968),#8328,.F.);
#8690=ADVANCED_FACE('',(#969),#8329,.F.);
#8691=ADVANCED_FACE('',(#970),#8330,.F.);
#8692=ADVANCED_FACE('',(#971),#8331,.F.);
#8693=ADVANCED_FACE('',(#972),#8332,.F.);
#8694=ADVANCED_FACE('',(#973),#8333,.F.);
#8695=ADVANCED_FACE('',(#974),#8334,.F.);
#8696=ADVANCED_FACE('',(#975),#8335,.F.);
#8697=ADVANCED_FACE('',(#976),#8336,.F.);
#8698=ADVANCED_FACE('',(#977),#8337,.F.);
#8699=ADVANCED_FACE('',(#978),#8338,.F.);
#8700=ADVANCED_FACE('',(#979),#8339,.F.);
#8701=ADVANCED_FACE('',(#980),#8340,.F.);
#8702=ADVANCED_FACE('',(#981),#8341,.F.);
#8703=ADVANCED_FACE('',(#982),#150,.F.);
#8704=ADVANCED_FACE('',(#983),#151,.F.);
#8705=ADVANCED_FACE('',(#984),#152,.F.);
#8706=ADVANCED_FACE('',(#985),#153,.F.);
#8707=ADVANCED_FACE('',(#986),#154,.F.);
#8708=ADVANCED_FACE('',(#987),#155,.F.);
#8709=ADVANCED_FACE('',(#988),#156,.F.);
#8710=ADVANCED_FACE('',(#989),#157,.F.);
#8711=ADVANCED_FACE('',(#990),#158,.F.);
#8712=ADVANCED_FACE('',(#991),#159,.F.);
#8713=ADVANCED_FACE('',(#992),#160,.F.);
#8714=ADVANCED_FACE('',(#993),#8342,.T.);
#8715=ADVANCED_FACE('',(#994),#8343,.F.);
#8716=ADVANCED_FACE('',(#995),#8344,.F.);
#8717=ADVANCED_FACE('',(#996),#8345,.F.);
#8718=ADVANCED_FACE('',(#997),#8346,.F.);
#8719=ADVANCED_FACE('',(#998),#8347,.F.);
#8720=ADVANCED_FACE('',(#999),#8348,.F.);
#8721=ADVANCED_FACE('',(#1000),#8349,.F.);
#8722=ADVANCED_FACE('',(#1001),#8350,.F.);
#8723=ADVANCED_FACE('',(#1002),#8351,.F.);
#8724=ADVANCED_FACE('',(#1003),#8352,.F.);
#8725=ADVANCED_FACE('',(#1004),#8353,.F.);
#8726=ADVANCED_FACE('',(#1005),#161,.F.);
#8727=ADVANCED_FACE('',(#1006),#162,.F.);
#8728=ADVANCED_FACE('',(#1007),#163,.F.);
#8729=ADVANCED_FACE('',(#1008),#164,.F.);
#8730=ADVANCED_FACE('',(#1009),#165,.F.);
#8731=ADVANCED_FACE('',(#1010),#166,.F.);
#8732=ADVANCED_FACE('',(#1011),#167,.F.);
#8733=ADVANCED_FACE('',(#1012),#168,.F.);
#8734=ADVANCED_FACE('',(#1013),#169,.F.);
#8735=ADVANCED_FACE('',(#1014),#170,.F.);
#8736=ADVANCED_FACE('',(#1015),#171,.F.);
#8737=ADVANCED_FACE('',(#1016),#8354,.T.);
#8738=ADVANCED_FACE('',(#1017),#8355,.F.);
#8739=ADVANCED_FACE('',(#1018),#8356,.F.);
#8740=ADVANCED_FACE('',(#1019),#8357,.F.);
#8741=ADVANCED_FACE('',(#1020),#8358,.F.);
#8742=ADVANCED_FACE('',(#1021),#8359,.F.);
#8743=ADVANCED_FACE('',(#1022),#8360,.F.);
#8744=ADVANCED_FACE('',(#1023),#8361,.F.);
#8745=ADVANCED_FACE('',(#1024),#8362,.F.);
#8746=ADVANCED_FACE('',(#1025),#8363,.F.);
#8747=ADVANCED_FACE('',(#1026),#8364,.F.);
#8748=ADVANCED_FACE('',(#1027),#8365,.F.);
#8749=ADVANCED_FACE('',(#1028),#172,.F.);
#8750=ADVANCED_FACE('',(#1029),#173,.F.);
#8751=ADVANCED_FACE('',(#1030),#174,.F.);
#8752=ADVANCED_FACE('',(#1031),#175,.F.);
#8753=ADVANCED_FACE('',(#1032),#176,.F.);
#8754=ADVANCED_FACE('',(#1033),#177,.F.);
#8755=ADVANCED_FACE('',(#1034),#178,.F.);
#8756=ADVANCED_FACE('',(#1035),#179,.F.);
#8757=ADVANCED_FACE('',(#1036),#180,.F.);
#8758=ADVANCED_FACE('',(#1037),#181,.F.);
#8759=ADVANCED_FACE('',(#1038),#182,.F.);
#8760=ADVANCED_FACE('',(#1039),#8366,.T.);
#8761=ADVANCED_FACE('',(#1040),#501,.F.);
#8762=ADVANCED_FACE('',(#1041),#502,.F.);
#8763=ADVANCED_FACE('',(#1042),#503,.F.);
#8764=ADVANCED_FACE('',(#1043),#504,.F.);
#8765=ADVANCED_FACE('',(#1044),#505,.F.);
#8766=ADVANCED_FACE('',(#1045),#506,.T.);
#8767=ADVANCED_FACE('',(#1046),#507,.T.);
#8768=ADVANCED_FACE('',(#1047),#8367,.T.);
#8769=ADVANCED_FACE('',(#1048),#8368,.T.);
#8770=ADVANCED_FACE('',(#1049),#392,.T.);
#8771=ADVANCED_FACE('',(#1050),#8369,.T.);
#8772=ADVANCED_FACE('',(#1051),#393,.T.);
#8773=ADVANCED_FACE('',(#1052),#8370,.T.);
#8774=ADVANCED_FACE('',(#1053),#394,.T.);
#8775=ADVANCED_FACE('',(#1054),#8371,.T.);
#8776=ADVANCED_FACE('',(#1055),#395,.T.);
#8777=ADVANCED_FACE('',(#1056),#508,.T.);
#8778=ADVANCED_FACE('',(#1057),#8372,.T.);
#8779=ADVANCED_FACE('',(#1058),#509,.T.);
#8780=ADVANCED_FACE('',(#1059),#8373,.T.);
#8781=ADVANCED_FACE('',(#1060,#598,#599,#600,#601,#602),#8374,.F.);
#8782=ADVANCED_FACE('',(#1061),#396,.F.);
#8783=ADVANCED_FACE('',(#1062,#603,#604,#605,#606,#607),#8375,.T.);
#8784=ADVANCED_FACE('',(#1063),#397,.F.);
#8785=ADVANCED_FACE('',(#1064),#8376,.T.);
#8786=ADVANCED_FACE('',(#1065),#398,.T.);
#8787=ADVANCED_FACE('',(#1066),#8377,.T.);
#8788=ADVANCED_FACE('',(#1067),#399,.T.);
#8789=ADVANCED_FACE('',(#1068),#8378,.T.);
#8790=ADVANCED_FACE('',(#1069),#400,.T.);
#8791=ADVANCED_FACE('',(#1070),#8379,.T.);
#8792=ADVANCED_FACE('',(#1071),#401,.T.);
#8793=ADVANCED_FACE('',(#1072),#8380,.T.);
#8794=ADVANCED_FACE('',(#1073),#510,.T.);
#8795=ADVANCED_FACE('',(#1074),#8381,.T.);
#8796=ADVANCED_FACE('',(#1075),#402,.F.);
#8797=ADVANCED_FACE('',(#1076),#403,.F.);
#8798=ADVANCED_FACE('',(#1077),#404,.F.);
#8799=ADVANCED_FACE('',(#1078),#405,.F.);
#8800=ADVANCED_FACE('',(#1079),#406,.F.);
#8801=ADVANCED_FACE('',(#1080),#407,.F.);
#8802=ADVANCED_FACE('',(#1081),#511,.F.);
#8803=ADVANCED_FACE('',(#1082),#512,.F.);
#8804=ADVANCED_FACE('',(#1083),#513,.F.);
#8805=ADVANCED_FACE('',(#1084),#514,.F.);
#8806=ADVANCED_FACE('',(#1085),#515,.F.);
#8807=ADVANCED_FACE('',(#1086),#516,.T.);
#8808=ADVANCED_FACE('',(#1087),#408,.F.);
#8809=ADVANCED_FACE('',(#1088,#608,#609),#8382,.F.);
#8810=ADVANCED_FACE('',(#1089),#517,.F.);
#8811=ADVANCED_FACE('',(#1090),#409,.F.);
#8812=ADVANCED_FACE('',(#1091),#518,.F.);
#8813=ADVANCED_FACE('',(#1092),#8383,.T.);
#8814=ADVANCED_FACE('',(#1093),#8384,.T.);
#8815=ADVANCED_FACE('',(#1094),#8385,.T.);
#8816=ADVANCED_FACE('',(#1095),#8386,.T.);
#8817=ADVANCED_FACE('',(#1096),#8387,.T.);
#8818=ADVANCED_FACE('',(#1097),#8388,.T.);
#8819=ADVANCED_FACE('',(#1098),#8389,.T.);
#8820=ADVANCED_FACE('',(#1099),#410,.F.);
#8821=ADVANCED_FACE('',(#1100,#610,#611),#8390,.T.);
#8822=ADVANCED_FACE('',(#1101),#519,.F.);
#8823=ADVANCED_FACE('',(#1102),#411,.F.);
#8824=ADVANCED_FACE('',(#1103),#520,.F.);
#8825=ADVANCED_FACE('',(#1104),#8391,.T.);
#8826=ADVANCED_FACE('',(#1105),#8392,.T.);
#8827=ADVANCED_FACE('',(#1106),#8393,.T.);
#8828=ADVANCED_FACE('',(#1107),#8394,.T.);
#8829=ADVANCED_FACE('',(#1108),#8395,.T.);
#8830=ADVANCED_FACE('',(#1109),#8396,.T.);
#8831=ADVANCED_FACE('',(#1110),#8397,.T.);
#8832=ADVANCED_FACE('',(#1111),#8398,.T.);
#8833=ADVANCED_FACE('',(#1112),#8399,.T.);
#8834=ADVANCED_FACE('',(#1113),#8400,.T.);
#8835=ADVANCED_FACE('',(#1114),#8401,.T.);
#8836=ADVANCED_FACE('',(#1115),#8402,.T.);
#8837=ADVANCED_FACE('',(#1116),#8403,.T.);
#8838=ADVANCED_FACE('',(#1117),#8404,.T.);
#8839=ADVANCED_FACE('',(#1118,#612,#613,#614),#8405,.T.);
#8840=ADVANCED_FACE('',(#1119),#521,.F.);
#8841=ADVANCED_FACE('',(#1120),#8406,.T.);
#8842=ADVANCED_FACE('',(#1121),#8407,.T.);
#8843=ADVANCED_FACE('',(#1122),#8408,.T.);
#8844=ADVANCED_FACE('',(#1123),#8409,.T.);
#8845=ADVANCED_FACE('',(#1124),#8410,.T.);
#8846=ADVANCED_FACE('',(#1125),#8411,.T.);
#8847=ADVANCED_FACE('',(#1126),#8412,.T.);
#8848=ADVANCED_FACE('',(#1127),#8413,.T.);
#8849=ADVANCED_FACE('',(#1128),#8414,.T.);
#8850=ADVANCED_FACE('',(#1129),#8415,.T.);
#8851=ADVANCED_FACE('',(#1130),#8416,.T.);
#8852=ADVANCED_FACE('',(#1131),#8417,.T.);
#8853=ADVANCED_FACE('',(#1132),#8418,.T.);
#8854=ADVANCED_FACE('',(#1133),#8419,.T.);
#8855=ADVANCED_FACE('',(#1134),#8420,.T.);
#8856=ADVANCED_FACE('',(#1135),#8421,.T.);
#8857=ADVANCED_FACE('',(#1136),#8422,.T.);
#8858=ADVANCED_FACE('',(#1137),#8423,.T.);
#8859=ADVANCED_FACE('',(#1138),#8424,.T.);
#8860=ADVANCED_FACE('',(#1139),#8425,.T.);
#8861=ADVANCED_FACE('',(#1140),#8426,.T.);
#8862=ADVANCED_FACE('',(#1141),#8427,.T.);
#8863=ADVANCED_FACE('',(#1142),#8428,.T.);
#8864=ADVANCED_FACE('',(#1143),#8429,.T.);
#8865=ADVANCED_FACE('',(#1144),#8430,.T.);
#8866=ADVANCED_FACE('',(#1145),#8431,.T.);
#8867=ADVANCED_FACE('',(#1146),#8432,.T.);
#8868=ADVANCED_FACE('',(#1147),#8433,.T.);
#8869=ADVANCED_FACE('',(#1148),#8434,.T.);
#8870=ADVANCED_FACE('',(#1149),#8435,.T.);
#8871=ADVANCED_FACE('',(#1150),#8436,.T.);
#8872=ADVANCED_FACE('',(#1151),#8437,.T.);
#8873=ADVANCED_FACE('',(#1152),#8438,.T.);
#8874=ADVANCED_FACE('',(#1153),#8439,.T.);
#8875=ADVANCED_FACE('',(#1154),#8440,.T.);
#8876=ADVANCED_FACE('',(#1155),#8441,.T.);
#8877=ADVANCED_FACE('',(#1156),#8442,.T.);
#8878=ADVANCED_FACE('',(#1157),#8443,.T.);
#8879=ADVANCED_FACE('',(#1158),#8444,.T.);
#8880=ADVANCED_FACE('',(#1159),#8445,.T.);
#8881=ADVANCED_FACE('',(#1160),#8446,.T.);
#8882=ADVANCED_FACE('',(#1161),#8447,.T.);
#8883=ADVANCED_FACE('',(#1162),#8448,.T.);
#8884=ADVANCED_FACE('',(#1163),#8449,.T.);
#8885=ADVANCED_FACE('',(#1164),#8450,.T.);
#8886=ADVANCED_FACE('',(#1165,#615,#616,#617),#8451,.T.);
#8887=ADVANCED_FACE('',(#1166),#8452,.T.);
#8888=ADVANCED_FACE('',(#1167),#8453,.F.);
#8889=ADVANCED_FACE('',(#1168),#8454,.F.);
#8890=ADVANCED_FACE('',(#1169),#8455,.F.);
#8891=ADVANCED_FACE('',(#1170),#8456,.T.);
#8892=ADVANCED_FACE('',(#1171),#8457,.T.);
#8893=ADVANCED_FACE('',(#1172),#8458,.T.);
#8894=ADVANCED_FACE('',(#1173),#8459,.T.);
#8895=ADVANCED_FACE('',(#1174),#8460,.T.);
#8896=ADVANCED_FACE('',(#1175),#8461,.T.);
#8897=ADVANCED_FACE('',(#1176),#8462,.F.);
#8898=ADVANCED_FACE('',(#1177),#8463,.F.);
#8899=ADVANCED_FACE('',(#1178),#522,.F.);
#8900=ADVANCED_FACE('',(#1179),#523,.F.);
#8901=ADVANCED_FACE('',(#1180),#524,.F.);
#8902=ADVANCED_FACE('',(#1181),#8464,.T.);
#8903=ADVANCED_FACE('',(#1182),#8465,.T.);
#8904=ADVANCED_FACE('',(#1183),#412,.T.);
#8905=ADVANCED_FACE('',(#1184),#525,.T.);
#8906=ADVANCED_FACE('',(#1185),#413,.T.);
#8907=ADVANCED_FACE('',(#1186),#8466,.T.);
#8908=ADVANCED_FACE('',(#1187),#414,.T.);
#8909=ADVANCED_FACE('',(#1188),#526,.T.);
#8910=ADVANCED_FACE('',(#1189),#8467,.T.);
#8911=ADVANCED_FACE('',(#1190),#8468,.T.);
#8912=ADVANCED_FACE('',(#1191),#415,.T.);
#8913=ADVANCED_FACE('',(#1192),#8469,.T.);
#8914=ADVANCED_FACE('',(#1193),#8470,.F.);
#8915=ADVANCED_FACE('',(#1194),#8471,.F.);
#8916=ADVANCED_FACE('',(#1195),#527,.T.);
#8917=ADVANCED_FACE('',(#1196,#618),#8472,.T.);
#8918=ADVANCED_FACE('',(#1197),#416,.T.);
#8919=ADVANCED_FACE('',(#1198),#417,.T.);
#8920=ADVANCED_FACE('',(#1199),#8473,.T.);
#8921=ADVANCED_FACE('',(#1200),#528,.T.);
#8922=ADVANCED_FACE('',(#1201),#418,.T.);
#8923=ADVANCED_FACE('',(#1202,#619),#8474,.T.);
#8924=ADVANCED_FACE('',(#1203),#529,.T.);
#8925=ADVANCED_FACE('',(#1204),#419,.T.);
#8926=ADVANCED_FACE('',(#1205),#8475,.T.);
#8927=ADVANCED_FACE('',(#1206),#420,.T.);
#8928=ADVANCED_FACE('',(#1207,#620),#8476,.T.);
#8929=ADVANCED_FACE('',(#1208),#530,.T.);
#8930=ADVANCED_FACE('',(#1209),#531,.F.);
#8931=ADVANCED_FACE('',(#1210,#621),#8477,.T.);
#8932=ADVANCED_FACE('',(#1211),#532,.T.);
#8933=ADVANCED_FACE('',(#1212,#622),#8478,.T.);
#8934=ADVANCED_FACE('',(#1213),#421,.T.);
#8935=ADVANCED_FACE('',(#1214),#8479,.T.);
#8936=ADVANCED_FACE('',(#1215),#8480,.F.);
#8937=ADVANCED_FACE('',(#1216),#422,.T.);
#8938=ADVANCED_FACE('',(#1217),#8481,.T.);
#8939=ADVANCED_FACE('',(#1218),#423,.T.);
#8940=ADVANCED_FACE('',(#1219),#8482,.T.);
#8941=ADVANCED_FACE('',(#1220),#8483,.F.);
#8942=ADVANCED_FACE('',(#1221),#424,.T.);
#8943=ADVANCED_FACE('',(#1222),#8484,.T.);
#8944=ADVANCED_FACE('',(#1223),#183,.T.);
#8945=ADVANCED_FACE('',(#1224),#533,.F.);
#8946=ADVANCED_FACE('',(#1225,#623),#534,.T.);
#8947=ADVANCED_FACE('',(#1226),#8485,.F.);
#8948=ADVANCED_FACE('',(#1227),#8486,.F.);
#8949=ADVANCED_FACE('',(#1228),#8487,.F.);
#8950=ADVANCED_FACE('',(#1229),#8488,.F.);
#8951=ADVANCED_FACE('',(#1230),#8489,.F.);
#8952=ADVANCED_FACE('',(#1231),#8490,.F.);
#8953=ADVANCED_FACE('',(#1232),#8491,.F.);
#8954=ADVANCED_FACE('',(#1233),#8492,.F.);
#8955=ADVANCED_FACE('',(#1234),#8493,.F.);
#8956=ADVANCED_FACE('',(#1235),#8494,.F.);
#8957=ADVANCED_FACE('',(#1236),#8495,.F.);
#8958=ADVANCED_FACE('',(#1237),#8496,.F.);
#8959=ADVANCED_FACE('',(#1238),#8497,.F.);
#8960=ADVANCED_FACE('',(#1239),#8498,.F.);
#8961=ADVANCED_FACE('',(#1240),#8499,.F.);
#8962=ADVANCED_FACE('',(#1241),#8500,.F.);
#8963=ADVANCED_FACE('',(#1242),#8501,.F.);
#8964=ADVANCED_FACE('',(#1243),#8502,.F.);
#8965=ADVANCED_FACE('',(#1244),#8503,.F.);
#8966=ADVANCED_FACE('',(#1245),#8504,.F.);
#8967=ADVANCED_FACE('',(#1246),#8505,.F.);
#8968=ADVANCED_FACE('',(#1247),#8506,.F.);
#8969=ADVANCED_FACE('',(#1248),#8507,.F.);
#8970=ADVANCED_FACE('',(#1249),#8508,.F.);
#8971=ADVANCED_FACE('',(#1250),#8509,.F.);
#8972=ADVANCED_FACE('',(#1251),#8510,.F.);
#8973=ADVANCED_FACE('',(#1252),#8511,.F.);
#8974=ADVANCED_FACE('',(#1253),#425,.T.);
#8975=ADVANCED_FACE('',(#1254),#8512,.T.);
#8976=ADVANCED_FACE('',(#1255),#8513,.T.);
#8977=ADVANCED_FACE('',(#1256),#8514,.T.);
#8978=ADVANCED_FACE('',(#1257),#8515,.T.);
#8979=ADVANCED_FACE('',(#1258),#8516,.T.);
#8980=ADVANCED_FACE('',(#1259),#8517,.T.);
#8981=ADVANCED_FACE('',(#1260),#8518,.T.);
#8982=ADVANCED_FACE('',(#1261),#8519,.T.);
#8983=ADVANCED_FACE('',(#1262),#8520,.T.);
#8984=ADVANCED_FACE('',(#1263),#8521,.T.);
#8985=ADVANCED_FACE('',(#1264),#8522,.T.);
#8986=ADVANCED_FACE('',(#1265),#8523,.T.);
#8987=ADVANCED_FACE('',(#1266),#426,.T.);
#8988=ADVANCED_FACE('',(#1267),#8524,.T.);
#8989=ADVANCED_FACE('',(#1268),#8525,.T.);
#8990=ADVANCED_FACE('',(#1269),#8526,.T.);
#8991=ADVANCED_FACE('',(#1270),#8527,.T.);
#8992=ADVANCED_FACE('',(#1271),#535,.T.);
#8993=ADVANCED_FACE('',(#1272),#8528,.T.);
#8994=ADVANCED_FACE('',(#1273),#536,.T.);
#8995=ADVANCED_FACE('',(#1274),#8529,.T.);
#8996=ADVANCED_FACE('',(#1275),#537,.T.);
#8997=ADVANCED_FACE('',(#1276),#8530,.T.);
#8998=ADVANCED_FACE('',(#1277),#427,.T.);
#8999=ADVANCED_FACE('',(#1278),#8531,.T.);
#9000=ADVANCED_FACE('',(#1279),#8532,.T.);
#9001=ADVANCED_FACE('',(#1280),#428,.T.);
#9002=ADVANCED_FACE('',(#1281),#8533,.T.);
#9003=ADVANCED_FACE('',(#1282),#8534,.T.);
#9004=ADVANCED_FACE('',(#1283),#538,.T.);
#9005=ADVANCED_FACE('',(#1284),#8535,.T.);
#9006=ADVANCED_FACE('',(#1285),#8536,.T.);
#9007=ADVANCED_FACE('',(#1286),#8537,.T.);
#9008=ADVANCED_FACE('',(#1287,#624),#539,.F.);
#9009=ADVANCED_FACE('',(#1288,#625),#8538,.T.);
#9010=ADVANCED_FACE('',(#1289),#429,.T.);
#9011=ADVANCED_FACE('',(#1290),#540,.T.);
#9012=ADVANCED_FACE('',(#1291),#541,.T.);
#9013=ADVANCED_FACE('',(#1292),#542,.T.);
#9014=ADVANCED_FACE('',(#1293),#543,.T.);
#9015=ADVANCED_FACE('',(#1294),#544,.T.);
#9016=ADVANCED_FACE('',(#1295),#545,.T.);
#9017=ADVANCED_FACE('',(#1296),#546,.T.);
#9018=ADVANCED_FACE('',(#1297),#547,.T.);
#9019=ADVANCED_FACE('',(#1298),#548,.T.);
#9020=ADVANCED_FACE('',(#1299),#549,.T.);
#9021=ADVANCED_FACE('',(#1300),#8539,.F.);
#9022=ADVANCED_FACE('',(#1301),#184,.F.);
#9023=ADVANCED_FACE('',(#1302),#8540,.T.);
#9024=ADVANCED_FACE('',(#1303),#550,.T.);
#9025=ADVANCED_FACE('',(#1304),#185,.F.);
#9026=ADVANCED_FACE('',(#1305),#8541,.F.);
#9027=ADVANCED_FACE('',(#1306),#8542,.F.);
#9028=ADVANCED_FACE('',(#1307),#8543,.F.);
#9029=ADVANCED_FACE('',(#1308),#8544,.F.);
#9030=ADVANCED_FACE('',(#1309),#8545,.F.);
#9031=ADVANCED_FACE('',(#1310),#8546,.F.);
#9032=ADVANCED_FACE('',(#1311),#8547,.F.);
#9033=ADVANCED_FACE('',(#1312),#8548,.T.);
#9034=ADVANCED_FACE('',(#1313),#430,.T.);
#9035=ADVANCED_FACE('',(#1314),#551,.T.);
#9036=ADVANCED_FACE('',(#1315),#431,.T.);
#9037=ADVANCED_FACE('',(#1316,#626),#8549,.T.);
#9038=ADVANCED_FACE('',(#1317),#552,.T.);
#9039=ADVANCED_FACE('',(#1318),#553,.T.);
#9040=ADVANCED_FACE('',(#1319),#554,.T.);
#9041=ADVANCED_FACE('',(#1320),#555,.T.);
#9042=ADVANCED_FACE('',(#1321),#556,.T.);
#9043=ADVANCED_FACE('',(#1322),#557,.T.);
#9044=ADVANCED_FACE('',(#1323),#558,.T.);
#9045=ADVANCED_FACE('',(#1324),#559,.T.);
#9046=ADVANCED_FACE('',(#1325),#560,.T.);
#9047=ADVANCED_FACE('',(#1326),#561,.T.);
#9048=ADVANCED_FACE('',(#1327),#562,.T.);
#9049=ADVANCED_FACE('',(#1328),#563,.T.);
#9050=ADVANCED_FACE('',(#1329),#564,.T.);
#9051=ADVANCED_FACE('',(#1330),#565,.T.);
#9052=ADVANCED_FACE('',(#1331),#566,.T.);
#9053=ADVANCED_FACE('',(#1332),#567,.T.);
#9054=ADVANCED_FACE('',(#1333),#568,.T.);
#9055=ADVANCED_FACE('',(#1334),#569,.T.);
#9056=ADVANCED_FACE('',(#1335),#570,.T.);
#9057=ADVANCED_FACE('',(#1336),#571,.T.);
#9058=ADVANCED_FACE('',(#1337),#572,.T.);
#9059=ADVANCED_FACE('',(#1338),#573,.T.);
#9060=ADVANCED_FACE('',(#1339),#574,.T.);
#9061=ADVANCED_FACE('',(#1340),#575,.T.);
#9062=ADVANCED_FACE('',(#1341),#8550,.F.);
#9063=ADVANCED_FACE('',(#1342),#186,.F.);
#9064=ADVANCED_FACE('',(#1343),#8551,.T.);
#9065=ADVANCED_FACE('',(#1344),#576,.T.);
#9066=ADVANCED_FACE('',(#1345),#187,.F.);
#9067=ADVANCED_FACE('',(#1346),#432,.F.);
#9068=ADVANCED_FACE('',(#1347),#8552,.F.);
#9069=ADVANCED_FACE('',(#1348),#8553,.F.);
#9070=ADVANCED_FACE('',(#1349),#8554,.F.);
#9071=ADVANCED_FACE('',(#1350),#8555,.F.);
#9072=ADVANCED_FACE('',(#1351),#8556,.F.);
#9073=ADVANCED_FACE('',(#1352),#8557,.F.);
#9074=ADVANCED_FACE('',(#1353,#627),#8558,.F.);
#9075=ADVANCED_FACE('',(#1354),#8559,.T.);
#9076=ADVANCED_FACE('',(#1355),#433,.T.);
#9077=ADVANCED_FACE('',(#1356),#577,.T.);
#9078=ADVANCED_FACE('',(#1357),#434,.T.);
#9079=ADVANCED_FACE('',(#1358,#628),#8560,.T.);
#9080=ADVANCED_FACE('',(#1359),#8561,.T.);
#9081=ADVANCED_FACE('',(#1360),#435,.T.);
#9082=ADVANCED_FACE('',(#1361),#578,.T.);
#9083=ADVANCED_FACE('',(#1362),#436,.T.);
#9084=ADVANCED_FACE('',(#1363),#8562,.T.);
#9085=CLOSED_SHELL('',(#8563,#8564,#8565,#8566,#8567,#8568,#8569,#8570,
#8571,#8572,#8573,#8574,#8575,#8576,#8577,#8578,#8579,#8580,#8581,#8582,
#8583));
#9086=CLOSED_SHELL('',(#8584,#8585,#8586,#8587,#8588,#8589,#8590,#8591,
#8592,#8593,#8594,#8595,#8596,#8597,#8598,#8599,#8600,#8601));
#9087=CLOSED_SHELL('',(#8602,#8603,#8604,#8605,#8606,#8607,#8608,#8609,
#8610,#8611,#8612,#8613,#8614,#8615,#8616,#8617,#8618,#8619,#8620,#8621,
#8622,#8623,#8624,#8625,#8626,#8627,#8628,#8629,#8630,#8631,#8632,#8633,
#8634,#8635,#8636,#8637,#8638,#8639,#8640,#8641,#8642,#8643,#8644,#8645,
#8646,#8647,#8648,#8649,#8650,#8651,#8652,#8653,#8654,#8655,#8656,#8657,
#8658,#8659,#8660,#8661,#8662,#8663,#8664,#8665,#8666,#8667,#8668,#8669,
#8670,#8671,#8672,#8673,#8674,#8675,#8676,#8677,#8678,#8679,#8680,#8681,
#8682,#8683,#8684,#8685,#8686,#8687,#8688,#8689,#8690,#8691,#8692,#8693,
#8694,#8695,#8696,#8697,#8698,#8699,#8700,#8701,#8702,#8703,#8704,#8705,
#8706,#8707,#8708,#8709,#8710,#8711,#8712,#8713,#8714,#8715,#8716,#8717,
#8718,#8719,#8720,#8721,#8722,#8723,#8724,#8725,#8726,#8727,#8728,#8729,
#8730,#8731,#8732,#8733,#8734,#8735,#8736,#8737,#8738,#8739,#8740,#8741,
#8742,#8743,#8744,#8745,#8746,#8747,#8748,#8749,#8750,#8751,#8752,#8753,
#8754,#8755,#8756,#8757,#8758,#8759,#8760,#8761,#8762,#8763,#8764,#8765,
#8766,#8767,#8768));
#9088=CLOSED_SHELL('',(#8769,#8770,#8771,#8772,#8773,#8774,#8775,#8776,
#8777,#8778,#8779,#8780,#8781,#8782,#8783,#8784,#8785,#8786,#8787,#8788,
#8789,#8790,#8791,#8792,#8793,#8794,#8795,#8796,#8797,#8798,#8799,#8800,
#8801,#8802,#8803,#8804,#8805,#8806,#8807));
#9089=CLOSED_SHELL('',(#8808,#8809,#8810,#8811,#8812,#8813,#8814,#8815,
#8816,#8817,#8818,#8819,#8820,#8821,#8822,#8823,#8824,#8825,#8826,#8827,
#8828,#8829,#8830,#8831,#8832,#8833,#8834,#8835,#8836,#8837,#8838,#8839,
#8840,#8841,#8842,#8843,#8844,#8845,#8846,#8847,#8848,#8849,#8850,#8851,
#8852,#8853,#8854,#8855,#8856,#8857,#8858,#8859,#8860,#8861,#8862,#8863,
#8864,#8865,#8866,#8867,#8868,#8869,#8870,#8871,#8872,#8873,#8874,#8875,
#8876,#8877,#8878,#8879,#8880,#8881,#8882,#8883,#8884,#8885,#8886,#8887,
#8888,#8889,#8890,#8891,#8892,#8893,#8894,#8895,#8896,#8897,#8898,#8899,
#8900,#8901,#8902));
#9090=CLOSED_SHELL('',(#8903,#8904,#8905,#8906,#8907));
#9091=CLOSED_SHELL('',(#8908,#8909,#8910,#8911,#8912,#8913,#8914,#8915,
#8916,#8917,#8918));
#9092=CLOSED_SHELL('',(#8919,#8920,#8921,#8922,#8923,#8924,#8925,#8926));
#9093=CLOSED_SHELL('',(#8927,#8928,#8929,#8930,#8931,#8932,#8933));
#9094=CLOSED_SHELL('',(#8934,#8935,#8936,#8937,#8938,#8939,#8940,#8941,
#8942,#8943,#8944,#8945,#8946,#8947,#8948,#8949,#8950,#8951,#8952,#8953,
#8954,#8955,#8956,#8957,#8958,#8959,#8960,#8961,#8962,#8963,#8964,#8965,
#8966,#8967,#8968,#8969,#8970,#8971,#8972,#8973,#8974,#8975,#8976,#8977,
#8978,#8979,#8980,#8981,#8982,#8983,#8984,#8985,#8986,#8987,#8988,#8989,
#8990,#8991,#8992,#8993,#8994,#8995,#8996,#8997,#8998,#8999,#9000,#9001,
#9002,#9003,#9004,#9005,#9006,#9007,#9008,#9009,#9010));
#9095=CLOSED_SHELL('',(#9011,#9012,#9013,#9014,#9015,#9016,#9017,#9018,
#9019,#9020,#9021,#9022,#9023,#9024,#9025,#9026,#9027,#9028,#9029,#9030,
#9031,#9032,#9033,#9034,#9035,#9036,#9037));
#9096=CLOSED_SHELL('',(#9038,#9039,#9040,#9041,#9042,#9043,#9044,#9045,
#9046,#9047,#9048,#9049,#9050,#9051,#9052,#9053,#9054,#9055,#9056,#9057,
#9058,#9059,#9060,#9061,#9062,#9063,#9064,#9065,#9066,#9067,#9068,#9069,
#9070,#9071,#9072,#9073,#9074,#9075,#9076,#9077,#9078,#9079));
#9097=CLOSED_SHELL('',(#9080,#9081,#9082,#9083,#9084));
#9098=DERIVED_UNIT_ELEMENT(#9124,1.);
#9099=DERIVED_UNIT_ELEMENT(#18283,-3.);
#9100=DERIVED_UNIT_ELEMENT(#9124,1.);
#9101=DERIVED_UNIT_ELEMENT(#18283,-3.);
#9102=DERIVED_UNIT_ELEMENT(#9124,1.);
#9103=DERIVED_UNIT_ELEMENT(#18283,-3.);
#9104=DERIVED_UNIT_ELEMENT(#9124,1.);
#9105=DERIVED_UNIT_ELEMENT(#18283,-3.);
#9106=DERIVED_UNIT_ELEMENT(#9124,1.);
#9107=DERIVED_UNIT_ELEMENT(#18283,-3.);
#9108=DERIVED_UNIT_ELEMENT(#9124,1.);
#9109=DERIVED_UNIT_ELEMENT(#18283,-3.);
#9110=DERIVED_UNIT_ELEMENT(#9124,1.);
#9111=DERIVED_UNIT_ELEMENT(#18283,-3.);
#9112=DERIVED_UNIT_ELEMENT(#9124,1.);
#9113=DERIVED_UNIT_ELEMENT(#18283,-3.);
#9114=DERIVED_UNIT_ELEMENT(#9124,1.);
#9115=DERIVED_UNIT_ELEMENT(#18283,-3.);
#9116=DERIVED_UNIT_ELEMENT(#9124,1.);
#9117=DERIVED_UNIT_ELEMENT(#18283,-3.);
#9118=DERIVED_UNIT_ELEMENT(#9124,1.);
#9119=DERIVED_UNIT_ELEMENT(#18283,-3.);
#9120=DERIVED_UNIT_ELEMENT(#9124,1.);
#9121=DERIVED_UNIT_ELEMENT(#18283,-3.);
#9122=DERIVED_UNIT_ELEMENT(#9124,1.);
#9123=DERIVED_UNIT_ELEMENT(#18283,-3.);
#9124=(
MASS_UNIT()
NAMED_UNIT(*)
SI_UNIT(.KILO.,.GRAM.)
);
#9125=DERIVED_UNIT((#9098,#9099));
#9126=DERIVED_UNIT((#9100,#9101));
#9127=DERIVED_UNIT((#9102,#9103));
#9128=DERIVED_UNIT((#9104,#9105));
#9129=DERIVED_UNIT((#9106,#9107));
#9130=DERIVED_UNIT((#9108,#9109));
#9131=DERIVED_UNIT((#9110,#9111));
#9132=DERIVED_UNIT((#9112,#9113));
#9133=DERIVED_UNIT((#9114,#9115));
#9134=DERIVED_UNIT((#9116,#9117));
#9135=DERIVED_UNIT((#9118,#9119));
#9136=DERIVED_UNIT((#9120,#9121));
#9137=DERIVED_UNIT((#9122,#9123));
#9138=MEASURE_REPRESENTATION_ITEM('density measure',
POSITIVE_RATIO_MEASURE(7850.),#9125);
#9139=MEASURE_REPRESENTATION_ITEM('density measure',
POSITIVE_RATIO_MEASURE(7850.),#9126);
#9140=MEASURE_REPRESENTATION_ITEM('density measure',
POSITIVE_RATIO_MEASURE(7850.),#9127);
#9141=MEASURE_REPRESENTATION_ITEM('density measure',
POSITIVE_RATIO_MEASURE(7850.),#9128);
#9142=MEASURE_REPRESENTATION_ITEM('density measure',
POSITIVE_RATIO_MEASURE(7850.),#9129);
#9143=MEASURE_REPRESENTATION_ITEM('density measure',
POSITIVE_RATIO_MEASURE(7850.),#9130);
#9144=MEASURE_REPRESENTATION_ITEM('density measure',
POSITIVE_RATIO_MEASURE(7850.),#9131);
#9145=MEASURE_REPRESENTATION_ITEM('density measure',
POSITIVE_RATIO_MEASURE(7850.),#9132);
#9146=MEASURE_REPRESENTATION_ITEM('density measure',
POSITIVE_RATIO_MEASURE(7850.),#9133);
#9147=MEASURE_REPRESENTATION_ITEM('density measure',
POSITIVE_RATIO_MEASURE(7850.),#9134);
#9148=MEASURE_REPRESENTATION_ITEM('density measure',
POSITIVE_RATIO_MEASURE(7850.),#9135);
#9149=MEASURE_REPRESENTATION_ITEM('density measure',
POSITIVE_RATIO_MEASURE(7850.),#9136);
#9150=MEASURE_REPRESENTATION_ITEM('density measure',
POSITIVE_RATIO_MEASURE(7850.),#9137);
#9151=PROPERTY_DEFINITION_REPRESENTATION(#9216,#9177);
#9152=PROPERTY_DEFINITION_REPRESENTATION(#9217,#9178);
#9153=PROPERTY_DEFINITION_REPRESENTATION(#9218,#9179);
#9154=PROPERTY_DEFINITION_REPRESENTATION(#9219,#9180);
#9155=PROPERTY_DEFINITION_REPRESENTATION(#9220,#9181);
#9156=PROPERTY_DEFINITION_REPRESENTATION(#9221,#9182);
#9157=PROPERTY_DEFINITION_REPRESENTATION(#9222,#9183);
#9158=PROPERTY_DEFINITION_REPRESENTATION(#9223,#9184);
#9159=PROPERTY_DEFINITION_REPRESENTATION(#9224,#9185);
#9160=PROPERTY_DEFINITION_REPRESENTATION(#9225,#9186);
#9161=PROPERTY_DEFINITION_REPRESENTATION(#9226,#9187);
#9162=PROPERTY_DEFINITION_REPRESENTATION(#9227,#9188);
#9163=PROPERTY_DEFINITION_REPRESENTATION(#9228,#9189);
#9164=PROPERTY_DEFINITION_REPRESENTATION(#9229,#9190);
#9165=PROPERTY_DEFINITION_REPRESENTATION(#9230,#9191);
#9166=PROPERTY_DEFINITION_REPRESENTATION(#9231,#9192);
#9167=PROPERTY_DEFINITION_REPRESENTATION(#9232,#9193);
#9168=PROPERTY_DEFINITION_REPRESENTATION(#9233,#9194);
#9169=PROPERTY_DEFINITION_REPRESENTATION(#9234,#9195);
#9170=PROPERTY_DEFINITION_REPRESENTATION(#9235,#9196);
#9171=PROPERTY_DEFINITION_REPRESENTATION(#9236,#9197);
#9172=PROPERTY_DEFINITION_REPRESENTATION(#9237,#9198);
#9173=PROPERTY_DEFINITION_REPRESENTATION(#9238,#9199);
#9174=PROPERTY_DEFINITION_REPRESENTATION(#9239,#9200);
#9175=PROPERTY_DEFINITION_REPRESENTATION(#9240,#9201);
#9176=PROPERTY_DEFINITION_REPRESENTATION(#9241,#9202);
#9177=REPRESENTATION('material name',(#9203),#18268);
#9178=REPRESENTATION('density',(#9138),#18268);
#9179=REPRESENTATION('material name',(#9204),#18269);
#9180=REPRESENTATION('density',(#9139),#18269);
#9181=REPRESENTATION('material name',(#9205),#18270);
#9182=REPRESENTATION('density',(#9140),#18270);
#9183=REPRESENTATION('material name',(#9206),#18271);
#9184=REPRESENTATION('density',(#9141),#18271);
#9185=REPRESENTATION('material name',(#9207),#18272);
#9186=REPRESENTATION('density',(#9142),#18272);
#9187=REPRESENTATION('material name',(#9208),#18273);
#9188=REPRESENTATION('density',(#9143),#18273);
#9189=REPRESENTATION('material name',(#9209),#18274);
#9190=REPRESENTATION('density',(#9144),#18274);
#9191=REPRESENTATION('material name',(#9210),#18275);
#9192=REPRESENTATION('density',(#9145),#18275);
#9193=REPRESENTATION('material name',(#9211),#18276);
#9194=REPRESENTATION('density',(#9146),#18276);
#9195=REPRESENTATION('material name',(#9212),#18277);
#9196=REPRESENTATION('density',(#9147),#18277);
#9197=REPRESENTATION('material name',(#9213),#18278);
#9198=REPRESENTATION('density',(#9148),#18278);
#9199=REPRESENTATION('material name',(#9214),#18279);
#9200=REPRESENTATION('density',(#9149),#18279);
#9201=REPRESENTATION('material name',(#9215),#18280);
#9202=REPRESENTATION('density',(#9150),#18280);
#9203=DESCRIPTIVE_REPRESENTATION_ITEM('Steel','Steel');
#9204=DESCRIPTIVE_REPRESENTATION_ITEM('Steel','Steel');
#9205=DESCRIPTIVE_REPRESENTATION_ITEM('Steel','Steel');
#9206=DESCRIPTIVE_REPRESENTATION_ITEM('Steel','Steel');
#9207=DESCRIPTIVE_REPRESENTATION_ITEM('Steel','Steel');
#9208=DESCRIPTIVE_REPRESENTATION_ITEM('Steel','Steel');
#9209=DESCRIPTIVE_REPRESENTATION_ITEM('Steel','Steel');
#9210=DESCRIPTIVE_REPRESENTATION_ITEM('Steel','Steel');
#9211=DESCRIPTIVE_REPRESENTATION_ITEM('Steel','Steel');
#9212=DESCRIPTIVE_REPRESENTATION_ITEM('Steel','Steel');
#9213=DESCRIPTIVE_REPRESENTATION_ITEM('Steel','Steel');
#9214=DESCRIPTIVE_REPRESENTATION_ITEM('Steel','Steel');
#9215=DESCRIPTIVE_REPRESENTATION_ITEM('Steel','Steel');
#9216=PROPERTY_DEFINITION('material property','material name',#18354);
#9217=PROPERTY_DEFINITION('material property','density of part',#18354);
#9218=PROPERTY_DEFINITION('material property','material name',#18355);
#9219=PROPERTY_DEFINITION('material property','density of part',#18355);
#9220=PROPERTY_DEFINITION('material property','material name',#18356);
#9221=PROPERTY_DEFINITION('material property','density of part',#18356);
#9222=PROPERTY_DEFINITION('material property','material name',#18357);
#9223=PROPERTY_DEFINITION('material property','density of part',#18357);
#9224=PROPERTY_DEFINITION('material property','material name',#18358);
#9225=PROPERTY_DEFINITION('material property','density of part',#18358);
#9226=PROPERTY_DEFINITION('material property','material name',#18359);
#9227=PROPERTY_DEFINITION('material property','density of part',#18359);
#9228=PROPERTY_DEFINITION('material property','material name',#18360);
#9229=PROPERTY_DEFINITION('material property','density of part',#18360);
#9230=PROPERTY_DEFINITION('material property','material name',#18361);
#9231=PROPERTY_DEFINITION('material property','density of part',#18361);
#9232=PROPERTY_DEFINITION('material property','material name',#18362);
#9233=PROPERTY_DEFINITION('material property','density of part',#18362);
#9234=PROPERTY_DEFINITION('material property','material name',#18363);
#9235=PROPERTY_DEFINITION('material property','density of part',#18363);
#9236=PROPERTY_DEFINITION('material property','material name',#18364);
#9237=PROPERTY_DEFINITION('material property','density of part',#18364);
#9238=PROPERTY_DEFINITION('material property','material name',#18365);
#9239=PROPERTY_DEFINITION('material property','density of part',#18365);
#9240=PROPERTY_DEFINITION('material property','material name',#18366);
#9241=PROPERTY_DEFINITION('material property','density of part',#18366);
#9242=AXIS2_PLACEMENT_3D('',#12271,#9970,#9971);
#9243=AXIS2_PLACEMENT_3D('',#12272,#9972,#9973);
#9244=AXIS2_PLACEMENT_3D('',#12273,#9974,#9975);
#9245=AXIS2_PLACEMENT_3D('',#12280,#9979,#9980);
#9246=AXIS2_PLACEMENT_3D('',#12287,#9984,#9985);
#9247=AXIS2_PLACEMENT_3D('',#12294,#9989,#9990);
#9248=AXIS2_PLACEMENT_3D('',#12301,#9994,#9995);
#9249=AXIS2_PLACEMENT_3D('',#12304,#9996,#9997);
#9250=AXIS2_PLACEMENT_3D('',#12307,#10000,#10001);
#9251=AXIS2_PLACEMENT_3D('',#12310,#10004,#10005);
#9252=AXIS2_PLACEMENT_3D('',#12313,#10008,#10009);
#9253=AXIS2_PLACEMENT_3D('',#12316,#10012,#10013);
#9254=AXIS2_PLACEMENT_3D('',#12319,#10014,#10015);
#9255=AXIS2_PLACEMENT_3D('',#12322,#10018,#10019);
#9256=AXIS2_PLACEMENT_3D('',#12325,#10020,#10021);
#9257=AXIS2_PLACEMENT_3D('',#12328,#10024,#10025);
#9258=AXIS2_PLACEMENT_3D('',#12331,#10028,#10029);
#9259=AXIS2_PLACEMENT_3D('',#12334,#10030,#10031);
#9260=AXIS2_PLACEMENT_3D('',#12337,#10034,#10035);
#9261=AXIS2_PLACEMENT_3D('',#12340,#10037,#10038);
#9262=AXIS2_PLACEMENT_3D('',#12342,#10039,#10040);
#9263=AXIS2_PLACEMENT_3D('',#12344,#10041,#10042);
#9264=AXIS2_PLACEMENT_3D('',#12345,#10043,#10044);
#9265=AXIS2_PLACEMENT_3D('',#12346,#10045,#10046);
#9266=AXIS2_PLACEMENT_3D('',#12347,#10047,#10048);
#9267=AXIS2_PLACEMENT_3D('',#12348,#10049,#10050);
#9268=AXIS2_PLACEMENT_3D('',#12350,#10051,#10052);
#9269=AXIS2_PLACEMENT_3D('',#12352,#10054,#10055);
#9270=AXIS2_PLACEMENT_3D('',#12354,#10056,#10057);
#9271=AXIS2_PLACEMENT_3D('',#12356,#10059,#10060);
#9272=AXIS2_PLACEMENT_3D('',#12358,#10061,#10062);
#9273=AXIS2_PLACEMENT_3D('',#12360,#10064,#10065);
#9274=AXIS2_PLACEMENT_3D('',#12362,#10067,#10068);
#9275=AXIS2_PLACEMENT_3D('',#12363,#10069,#10070);
#9276=AXIS2_PLACEMENT_3D('',#12364,#10071,#10072);
#9277=AXIS2_PLACEMENT_3D('',#12365,#10073,#10074);
#9278=AXIS2_PLACEMENT_3D('',#12366,#10075,#10076);
#9279=AXIS2_PLACEMENT_3D('',#12373,#10080,#10081);
#9280=AXIS2_PLACEMENT_3D('',#12380,#10085,#10086);
#9281=AXIS2_PLACEMENT_3D('',#12383,#10087,#10088);
#9282=AXIS2_PLACEMENT_3D('',#12386,#10091,#10092);
#9283=AXIS2_PLACEMENT_3D('',#12389,#10095,#10096);
#9284=AXIS2_PLACEMENT_3D('',#12396,#10100,#10101);
#9285=AXIS2_PLACEMENT_3D('',#12403,#10105,#10106);
#9286=AXIS2_PLACEMENT_3D('',#12406,#10107,#10108);
#9287=AXIS2_PLACEMENT_3D('',#12409,#10111,#10112);
#9288=AXIS2_PLACEMENT_3D('',#12412,#10115,#10116);
#9289=AXIS2_PLACEMENT_3D('',#12415,#10119,#10120);
#9290=AXIS2_PLACEMENT_3D('',#12418,#10123,#10124);
#9291=AXIS2_PLACEMENT_3D('',#12421,#10125,#10126);
#9292=AXIS2_PLACEMENT_3D('',#12424,#10129,#10130);
#9293=AXIS2_PLACEMENT_3D('',#12427,#10131,#10132);
#9294=AXIS2_PLACEMENT_3D('',#12430,#10135,#10136);
#9295=AXIS2_PLACEMENT_3D('',#12432,#10138,#10139);
#9296=AXIS2_PLACEMENT_3D('',#12433,#10140,#10141);
#9297=AXIS2_PLACEMENT_3D('',#12434,#10142,#10143);
#9298=AXIS2_PLACEMENT_3D('',#12435,#10144,#10145);
#9299=AXIS2_PLACEMENT_3D('',#12437,#10147,#10148);
#9300=AXIS2_PLACEMENT_3D('',#12438,#10149,#10150);
#9301=AXIS2_PLACEMENT_3D('',#12439,#10151,#10152);
#9302=AXIS2_PLACEMENT_3D('',#12440,#10153,#10154);
#9303=AXIS2_PLACEMENT_3D('',#12441,#10155,#10156);
#9304=AXIS2_PLACEMENT_3D('',#12450,#10161,#10162);
#9305=AXIS2_PLACEMENT_3D('',#12452,#10163,#10164);
#9306=AXIS2_PLACEMENT_3D('',#12455,#10166,#10167);
#9307=AXIS2_PLACEMENT_3D('',#12456,#10168,#10169);
#9308=AXIS2_PLACEMENT_3D('',#12462,#10173,#10174);
#9309=AXIS2_PLACEMENT_3D('',#12464,#10175,#10176);
#9310=AXIS2_PLACEMENT_3D('',#12467,#10178,#10179);
#9311=AXIS2_PLACEMENT_3D('',#12468,#10180,#10181);
#9312=AXIS2_PLACEMENT_3D('',#12474,#10185,#10186);
#9313=AXIS2_PLACEMENT_3D('',#12476,#10187,#10188);
#9314=AXIS2_PLACEMENT_3D('',#12479,#10190,#10191);
#9315=AXIS2_PLACEMENT_3D('',#12480,#10192,#10193);
#9316=AXIS2_PLACEMENT_3D('',#12486,#10197,#10198);
#9317=AXIS2_PLACEMENT_3D('',#12487,#10199,#10200);
#9318=AXIS2_PLACEMENT_3D('',#12488,#10201,#10202);
#9319=AXIS2_PLACEMENT_3D('',#12489,#10203,#10204);
#9320=AXIS2_PLACEMENT_3D('',#12493,#10206,#10207);
#9321=AXIS2_PLACEMENT_3D('',#12495,#10209,#10210);
#9322=AXIS2_PLACEMENT_3D('',#12499,#10213,#10214);
#9323=AXIS2_PLACEMENT_3D('',#12502,#10216,#10217);
#9324=AXIS2_PLACEMENT_3D('',#12503,#10218,#10219);
#9325=AXIS2_PLACEMENT_3D('',#12507,#10222,#10223);
#9326=AXIS2_PLACEMENT_3D('',#12509,#10224,#10225);
#9327=AXIS2_PLACEMENT_3D('',#12511,#10226,#10227);
#9328=AXIS2_PLACEMENT_3D('',#12513,#10228,#10229);
#9329=AXIS2_PLACEMENT_3D('',#12515,#10230,#10231);
#9330=AXIS2_PLACEMENT_3D('',#12517,#10232,#10233);
#9331=AXIS2_PLACEMENT_3D('',#12518,#10234,#10235);
#9332=AXIS2_PLACEMENT_3D('',#12526,#10240,#10241);
#9333=AXIS2_PLACEMENT_3D('',#12529,#10243,#10244);
#9334=AXIS2_PLACEMENT_3D('',#12530,#10245,#10246);
#9335=AXIS2_PLACEMENT_3D('',#12534,#10249,#10250);
#9336=AXIS2_PLACEMENT_3D('',#12537,#10252,#10253);
#9337=AXIS2_PLACEMENT_3D('',#12538,#10254,#10255);
#9338=AXIS2_PLACEMENT_3D('',#12542,#10258,#10259);
#9339=AXIS2_PLACEMENT_3D('',#12546,#10261,#10262);
#9340=AXIS2_PLACEMENT_3D('',#12547,#10263,#10264);
#9341=AXIS2_PLACEMENT_3D('',#12548,#10265,#10266);
#9342=AXIS2_PLACEMENT_3D('',#12568,#10272,#10273);
#9343=AXIS2_PLACEMENT_3D('',#12569,#10274,#10275);
#9344=AXIS2_PLACEMENT_3D('',#12570,#10276,#10277);
#9345=AXIS2_PLACEMENT_3D('',#12571,#10278,#10279);
#9346=AXIS2_PLACEMENT_3D('',#12573,#10281,#10282);
#9347=AXIS2_PLACEMENT_3D('',#12577,#10284,#10285);
#9348=AXIS2_PLACEMENT_3D('',#12579,#10287,#10288);
#9349=AXIS2_PLACEMENT_3D('',#12583,#10291,#10292);
#9350=AXIS2_PLACEMENT_3D('',#12586,#10294,#10295);
#9351=AXIS2_PLACEMENT_3D('',#12587,#10296,#10297);
#9352=AXIS2_PLACEMENT_3D('',#12623,#10308,#10309);
#9353=AXIS2_PLACEMENT_3D('',#12674,#10312,#10313);
#9354=AXIS2_PLACEMENT_3D('',#12687,#10315,#10316);
#9355=AXIS2_PLACEMENT_3D('',#12689,#10317,#10318);
#9356=AXIS2_PLACEMENT_3D('',#12693,#10320,#10321);
#9357=AXIS2_PLACEMENT_3D('',#12713,#10322,#10323);
#9358=AXIS2_PLACEMENT_3D('',#12714,#10324,#10325);
#9359=AXIS2_PLACEMENT_3D('',#12717,#10327,#10328);
#9360=AXIS2_PLACEMENT_3D('',#12719,#10330,#10331);
#9361=AXIS2_PLACEMENT_3D('',#12727,#10336,#10337);
#9362=AXIS2_PLACEMENT_3D('',#12730,#10339,#10340);
#9363=AXIS2_PLACEMENT_3D('',#12731,#10341,#10342);
#9364=AXIS2_PLACEMENT_3D('',#12733,#10343,#10344);
#9365=AXIS2_PLACEMENT_3D('',#12737,#10346,#10347);
#9366=AXIS2_PLACEMENT_3D('',#12757,#10348,#10349);
#9367=AXIS2_PLACEMENT_3D('',#12758,#10350,#10351);
#9368=AXIS2_PLACEMENT_3D('',#12761,#10354,#10355);
#9369=AXIS2_PLACEMENT_3D('',#12769,#10358,#10359);
#9370=AXIS2_PLACEMENT_3D('',#12772,#10361,#10362);
#9371=AXIS2_PLACEMENT_3D('',#12773,#10363,#10364);
#9372=AXIS2_PLACEMENT_3D('',#12775,#10365,#10366);
#9373=AXIS2_PLACEMENT_3D('',#12783,#10368,#10369);
#9374=AXIS2_PLACEMENT_3D('',#12802,#10370,#10371);
#9375=AXIS2_PLACEMENT_3D('',#12807,#10375,#10376);
#9376=AXIS2_PLACEMENT_3D('',#12810,#10378,#10379);
#9377=AXIS2_PLACEMENT_3D('',#13013,#10426,#10427);
#9378=AXIS2_PLACEMENT_3D('',#13078,#10438,#10439);
#9379=AXIS2_PLACEMENT_3D('',#13081,#10441,#10442);
#9380=AXIS2_PLACEMENT_3D('',#13082,#10443,#10444);
#9381=AXIS2_PLACEMENT_3D('',#13084,#10445,#10446);
#9382=AXIS2_PLACEMENT_3D('',#13104,#10448,#10449);
#9383=AXIS2_PLACEMENT_3D('',#13107,#10451,#10452);
#9384=AXIS2_PLACEMENT_3D('',#13108,#10453,#10454);
#9385=AXIS2_PLACEMENT_3D('',#13115,#10459,#10460);
#9386=AXIS2_PLACEMENT_3D('',#13119,#10463,#10464);
#9387=AXIS2_PLACEMENT_3D('',#13123,#10467,#10468);
#9388=AXIS2_PLACEMENT_3D('',#13124,#10469,#10470);
#9389=AXIS2_PLACEMENT_3D('',#13126,#10472,#10473);
#9390=AXIS2_PLACEMENT_3D('',#13130,#10476,#10477);
#9391=AXIS2_PLACEMENT_3D('',#13131,#10478,#10479);
#9392=AXIS2_PLACEMENT_3D('',#13132,#10480,#10481);
#9393=AXIS2_PLACEMENT_3D('',#13134,#10483,#10484);
#9394=AXIS2_PLACEMENT_3D('',#13136,#10486,#10487);
#9395=AXIS2_PLACEMENT_3D('',#13138,#10489,#10490);
#9396=AXIS2_PLACEMENT_3D('',#13139,#10491,#10492);
#9397=AXIS2_PLACEMENT_3D('',#13143,#10495,#10496);
#9398=AXIS2_PLACEMENT_3D('',#13147,#10499,#10500);
#9399=AXIS2_PLACEMENT_3D('',#13171,#10501,#10502);
#9400=AXIS2_PLACEMENT_3D('',#13175,#10505,#10506);
#9401=AXIS2_PLACEMENT_3D('',#13179,#10509,#10510);
#9402=AXIS2_PLACEMENT_3D('',#13183,#10513,#10514);
#9403=AXIS2_PLACEMENT_3D('',#13187,#10517,#10518);
#9404=AXIS2_PLACEMENT_3D('',#13191,#10521,#10522);
#9405=AXIS2_PLACEMENT_3D('',#13195,#10525,#10526);
#9406=AXIS2_PLACEMENT_3D('',#13197,#10528,#10529);
#9407=AXIS2_PLACEMENT_3D('',#13198,#10530,#10531);
#9408=AXIS2_PLACEMENT_3D('',#13202,#10534,#10535);
#9409=AXIS2_PLACEMENT_3D('',#13206,#10538,#10539);
#9410=AXIS2_PLACEMENT_3D('',#13210,#10542,#10543);
#9411=AXIS2_PLACEMENT_3D('',#13214,#10546,#10547);
#9412=AXIS2_PLACEMENT_3D('',#13218,#10550,#10551);
#9413=AXIS2_PLACEMENT_3D('',#13222,#10554,#10555);
#9414=AXIS2_PLACEMENT_3D('',#13224,#10557,#10558);
#9415=AXIS2_PLACEMENT_3D('',#13274,#10564,#10565);
#9416=AXIS2_PLACEMENT_3D('',#13280,#10569,#10570);
#9417=AXIS2_PLACEMENT_3D('',#13284,#10573,#10574);
#9418=AXIS2_PLACEMENT_3D('',#13288,#10577,#10578);
#9419=AXIS2_PLACEMENT_3D('',#13292,#10581,#10582);
#9420=AXIS2_PLACEMENT_3D('',#13296,#10585,#10586);
#9421=AXIS2_PLACEMENT_3D('',#13300,#10589,#10590);
#9422=AXIS2_PLACEMENT_3D('',#13304,#10593,#10594);
#9423=AXIS2_PLACEMENT_3D('',#13308,#10597,#10598);
#9424=AXIS2_PLACEMENT_3D('',#13312,#10601,#10602);
#9425=AXIS2_PLACEMENT_3D('',#13314,#10604,#10605);
#9426=AXIS2_PLACEMENT_3D('',#13315,#10606,#10607);
#9427=AXIS2_PLACEMENT_3D('',#13321,#10611,#10612);
#9428=AXIS2_PLACEMENT_3D('',#13325,#10615,#10616);
#9429=AXIS2_PLACEMENT_3D('',#13329,#10619,#10620);
#9430=AXIS2_PLACEMENT_3D('',#13333,#10623,#10624);
#9431=AXIS2_PLACEMENT_3D('',#13337,#10627,#10628);
#9432=AXIS2_PLACEMENT_3D('',#13341,#10631,#10632);
#9433=AXIS2_PLACEMENT_3D('',#13345,#10635,#10636);
#9434=AXIS2_PLACEMENT_3D('',#13349,#10639,#10640);
#9435=AXIS2_PLACEMENT_3D('',#13353,#10643,#10644);
#9436=AXIS2_PLACEMENT_3D('',#13355,#10646,#10647);
#9437=AXIS2_PLACEMENT_3D('',#13477,#10659,#10660);
#9438=AXIS2_PLACEMENT_3D('',#13478,#10661,#10662);
#9439=AXIS2_PLACEMENT_3D('',#13484,#10666,#10667);
#9440=AXIS2_PLACEMENT_3D('',#13488,#10670,#10671);
#9441=AXIS2_PLACEMENT_3D('',#13492,#10674,#10675);
#9442=AXIS2_PLACEMENT_3D('',#13496,#10678,#10679);
#9443=AXIS2_PLACEMENT_3D('',#13500,#10682,#10683);
#9444=AXIS2_PLACEMENT_3D('',#13504,#10686,#10687);
#9445=AXIS2_PLACEMENT_3D('',#13508,#10690,#10691);
#9446=AXIS2_PLACEMENT_3D('',#13512,#10694,#10695);
#9447=AXIS2_PLACEMENT_3D('',#13516,#10698,#10699);
#9448=AXIS2_PLACEMENT_3D('',#13518,#10701,#10702);
#9449=AXIS2_PLACEMENT_3D('',#13640,#10714,#10715);
#9450=AXIS2_PLACEMENT_3D('',#13641,#10716,#10717);
#9451=AXIS2_PLACEMENT_3D('',#13647,#10721,#10722);
#9452=AXIS2_PLACEMENT_3D('',#13651,#10725,#10726);
#9453=AXIS2_PLACEMENT_3D('',#13655,#10729,#10730);
#9454=AXIS2_PLACEMENT_3D('',#13659,#10733,#10734);
#9455=AXIS2_PLACEMENT_3D('',#13663,#10737,#10738);
#9456=AXIS2_PLACEMENT_3D('',#13667,#10741,#10742);
#9457=AXIS2_PLACEMENT_3D('',#13671,#10745,#10746);
#9458=AXIS2_PLACEMENT_3D('',#13675,#10749,#10750);
#9459=AXIS2_PLACEMENT_3D('',#13679,#10753,#10754);
#9460=AXIS2_PLACEMENT_3D('',#13681,#10756,#10757);
#9461=AXIS2_PLACEMENT_3D('',#13803,#10769,#10770);
#9462=AXIS2_PLACEMENT_3D('',#13804,#10771,#10772);
#9463=AXIS2_PLACEMENT_3D('',#13806,#10774,#10775);
#9464=AXIS2_PLACEMENT_3D('',#13808,#10777,#10778);
#9465=AXIS2_PLACEMENT_3D('',#13810,#10780,#10781);
#9466=AXIS2_PLACEMENT_3D('',#13812,#10783,#10784);
#9467=AXIS2_PLACEMENT_3D('',#13814,#10786,#10787);
#9468=AXIS2_PLACEMENT_3D('',#13816,#10789,#10790);
#9469=AXIS2_PLACEMENT_3D('',#13818,#10792,#10793);
#9470=AXIS2_PLACEMENT_3D('',#13819,#10794,#10795);
#9471=AXIS2_PLACEMENT_3D('',#13820,#10796,#10797);
#9472=AXIS2_PLACEMENT_3D('',#13829,#10802,#10803);
#9473=AXIS2_PLACEMENT_3D('',#13833,#10805,#10806);
#9474=AXIS2_PLACEMENT_3D('',#13834,#10807,#10808);
#9475=AXIS2_PLACEMENT_3D('',#13835,#10809,#10810);
#9476=AXIS2_PLACEMENT_3D('',#13841,#10814,#10815);
#9477=AXIS2_PLACEMENT_3D('',#13845,#10817,#10818);
#9478=AXIS2_PLACEMENT_3D('',#13846,#10819,#10820);
#9479=AXIS2_PLACEMENT_3D('',#13847,#10821,#10822);
#9480=AXIS2_PLACEMENT_3D('',#13853,#10826,#10827);
#9481=AXIS2_PLACEMENT_3D('',#13857,#10829,#10830);
#9482=AXIS2_PLACEMENT_3D('',#13858,#10831,#10832);
#9483=AXIS2_PLACEMENT_3D('',#13859,#10833,#10834);
#9484=AXIS2_PLACEMENT_3D('',#13865,#10838,#10839);
#9485=AXIS2_PLACEMENT_3D('',#13866,#10840,#10841);
#9486=AXIS2_PLACEMENT_3D('',#13867,#10842,#10843);
#9487=AXIS2_PLACEMENT_3D('',#13868,#10844,#10845);
#9488=AXIS2_PLACEMENT_3D('',#13872,#10847,#10848);
#9489=AXIS2_PLACEMENT_3D('',#13874,#10850,#10851);
#9490=AXIS2_PLACEMENT_3D('',#13878,#10854,#10855);
#9491=AXIS2_PLACEMENT_3D('',#13881,#10857,#10858);
#9492=AXIS2_PLACEMENT_3D('',#13882,#10859,#10860);
#9493=AXIS2_PLACEMENT_3D('',#13886,#10863,#10864);
#9494=AXIS2_PLACEMENT_3D('',#13888,#10865,#10866);
#9495=AXIS2_PLACEMENT_3D('',#13890,#10867,#10868);
#9496=AXIS2_PLACEMENT_3D('',#13892,#10869,#10870);
#9497=AXIS2_PLACEMENT_3D('',#13894,#10871,#10872);
#9498=AXIS2_PLACEMENT_3D('',#13896,#10873,#10874);
#9499=AXIS2_PLACEMENT_3D('',#13897,#10875,#10876);
#9500=AXIS2_PLACEMENT_3D('',#13899,#10877,#10878);
#9501=AXIS2_PLACEMENT_3D('',#13902,#10880,#10881);
#9502=AXIS2_PLACEMENT_3D('',#13903,#10882,#10883);
#9503=AXIS2_PLACEMENT_3D('',#13908,#10885,#10886);
#9504=AXIS2_PLACEMENT_3D('',#13912,#10888,#10889);
#9505=AXIS2_PLACEMENT_3D('',#13916,#10891,#10892);
#9506=AXIS2_PLACEMENT_3D('',#13919,#10894,#10895);
#9507=AXIS2_PLACEMENT_3D('',#13921,#10896,#10897);
#9508=AXIS2_PLACEMENT_3D('',#13923,#10898,#10899);
#9509=AXIS2_PLACEMENT_3D('',#13925,#10900,#10901);
#9510=AXIS2_PLACEMENT_3D('',#13927,#10902,#10903);
#9511=AXIS2_PLACEMENT_3D('',#13928,#10904,#10905);
#9512=AXIS2_PLACEMENT_3D('',#13931,#10907,#10908);
#9513=AXIS2_PLACEMENT_3D('',#13932,#10909,#10910);
#9514=AXIS2_PLACEMENT_3D('',#13938,#10914,#10915);
#9515=AXIS2_PLACEMENT_3D('',#13940,#10916,#10917);
#9516=AXIS2_PLACEMENT_3D('',#13942,#10919,#10920);
#9517=AXIS2_PLACEMENT_3D('',#13945,#10923,#10924);
#9518=AXIS2_PLACEMENT_3D('',#13947,#10926,#10927);
#9519=AXIS2_PLACEMENT_3D('',#13949,#10929,#10930);
#9520=AXIS2_PLACEMENT_3D('',#13951,#10932,#10933);
#9521=AXIS2_PLACEMENT_3D('',#13953,#10935,#10936);
#9522=AXIS2_PLACEMENT_3D('',#13954,#10937,#10938);
#9523=AXIS2_PLACEMENT_3D('',#13955,#10939,#10940);
#9524=AXIS2_PLACEMENT_3D('',#13957,#10942,#10943);
#9525=AXIS2_PLACEMENT_3D('',#13959,#10945,#10946);
#9526=AXIS2_PLACEMENT_3D('',#13961,#10948,#10949);
#9527=AXIS2_PLACEMENT_3D('',#13963,#10950,#10951);
#9528=AXIS2_PLACEMENT_3D('',#13965,#10953,#10954);
#9529=AXIS2_PLACEMENT_3D('',#13968,#10956,#10957);
#9530=AXIS2_PLACEMENT_3D('',#13969,#10958,#10959);
#9531=AXIS2_PLACEMENT_3D('',#13971,#10960,#10961);
#9532=AXIS2_PLACEMENT_3D('',#13973,#10963,#10964);
#9533=AXIS2_PLACEMENT_3D('',#13976,#10966,#10967);
#9534=AXIS2_PLACEMENT_3D('',#13977,#10968,#10969);
#9535=AXIS2_PLACEMENT_3D('',#13979,#10970,#10971);
#9536=AXIS2_PLACEMENT_3D('',#13981,#10973,#10974);
#9537=AXIS2_PLACEMENT_3D('',#13984,#10976,#10977);
#9538=AXIS2_PLACEMENT_3D('',#13985,#10978,#10979);
#9539=AXIS2_PLACEMENT_3D('',#13987,#10981,#10982);
#9540=AXIS2_PLACEMENT_3D('',#13989,#10984,#10985);
#9541=AXIS2_PLACEMENT_3D('',#13991,#10987,#10988);
#9542=AXIS2_PLACEMENT_3D('',#13993,#10990,#10991);
#9543=AXIS2_PLACEMENT_3D('',#13995,#10993,#10994);
#9544=AXIS2_PLACEMENT_3D('',#13996,#10995,#10996);
#9545=AXIS2_PLACEMENT_3D('',#13997,#10997,#10998);
#9546=AXIS2_PLACEMENT_3D('',#13999,#10999,#11000);
#9547=AXIS2_PLACEMENT_3D('',#14002,#11002,#11003);
#9548=AXIS2_PLACEMENT_3D('',#14003,#11004,#11005);
#9549=AXIS2_PLACEMENT_3D('',#14050,#11028,#11029);
#9550=AXIS2_PLACEMENT_3D('',#14053,#11031,#11032);
#9551=AXIS2_PLACEMENT_3D('',#14054,#11033,#11034);
#9552=AXIS2_PLACEMENT_3D('',#14057,#11036,#11037);
#9553=AXIS2_PLACEMENT_3D('',#14058,#11038,#11039);
#9554=AXIS2_PLACEMENT_3D('',#14061,#11041,#11042);
#9555=AXIS2_PLACEMENT_3D('',#14062,#11043,#11044);
#9556=AXIS2_PLACEMENT_3D('',#14065,#11046,#11047);
#9557=AXIS2_PLACEMENT_3D('',#14066,#11048,#11049);
#9558=AXIS2_PLACEMENT_3D('',#14079,#11056,#11057);
#9559=AXIS2_PLACEMENT_3D('',#14085,#11061,#11062);
#9560=AXIS2_PLACEMENT_3D('',#14093,#11067,#11068);
#9561=AXIS2_PLACEMENT_3D('',#14099,#11072,#11073);
#9562=AXIS2_PLACEMENT_3D('',#14107,#11078,#11079);
#9563=AXIS2_PLACEMENT_3D('',#14110,#11082,#11083);
#9564=AXIS2_PLACEMENT_3D('',#14114,#11086,#11087);
#9565=AXIS2_PLACEMENT_3D('',#14116,#11088,#11089);
#9566=AXIS2_PLACEMENT_3D('',#14119,#11091,#11092);
#9567=AXIS2_PLACEMENT_3D('',#14120,#11093,#11094);
#9568=AXIS2_PLACEMENT_3D('',#14124,#11096,#11097);
#9569=AXIS2_PLACEMENT_3D('',#14165,#11118,#11119);
#9570=AXIS2_PLACEMENT_3D('',#14166,#11120,#11121);
#9571=AXIS2_PLACEMENT_3D('',#14169,#11123,#11124);
#9572=AXIS2_PLACEMENT_3D('',#14170,#11125,#11126);
#9573=AXIS2_PLACEMENT_3D('',#14173,#11128,#11129);
#9574=AXIS2_PLACEMENT_3D('',#14174,#11130,#11131);
#9575=AXIS2_PLACEMENT_3D('',#14177,#11133,#11134);
#9576=AXIS2_PLACEMENT_3D('',#14178,#11135,#11136);
#9577=AXIS2_PLACEMENT_3D('',#14184,#11140,#11141);
#9578=AXIS2_PLACEMENT_3D('',#14186,#11143,#11144);
#9579=AXIS2_PLACEMENT_3D('',#14188,#11145,#11146);
#9580=AXIS2_PLACEMENT_3D('',#14190,#11148,#11149);
#9581=AXIS2_PLACEMENT_3D('',#14194,#11152,#11153);
#9582=AXIS2_PLACEMENT_3D('',#14197,#11156,#11157);
#9583=AXIS2_PLACEMENT_3D('',#14199,#11158,#11159);
#9584=AXIS2_PLACEMENT_3D('',#14201,#11161,#11162);
#9585=AXIS2_PLACEMENT_3D('',#14202,#11163,#11164);
#9586=AXIS2_PLACEMENT_3D('',#14208,#11168,#11169);
#9587=AXIS2_PLACEMENT_3D('',#14214,#11173,#11174);
#9588=AXIS2_PLACEMENT_3D('',#14220,#11178,#11179);
#9589=AXIS2_PLACEMENT_3D('',#14223,#11182,#11183);
#9590=AXIS2_PLACEMENT_3D('',#14229,#11187,#11188);
#9591=AXIS2_PLACEMENT_3D('',#14231,#11189,#11190);
#9592=AXIS2_PLACEMENT_3D('',#14233,#11192,#11193);
#9593=AXIS2_PLACEMENT_3D('',#14235,#11194,#11195);
#9594=AXIS2_PLACEMENT_3D('',#14237,#11197,#11198);
#9595=AXIS2_PLACEMENT_3D('',#14240,#11200,#11201);
#9596=AXIS2_PLACEMENT_3D('',#14242,#11202,#11203);
#9597=AXIS2_PLACEMENT_3D('',#14244,#11204,#11205);
#9598=AXIS2_PLACEMENT_3D('',#14245,#11206,#11207);
#9599=AXIS2_PLACEMENT_3D('',#14247,#11209,#11210);
#9600=AXIS2_PLACEMENT_3D('',#14251,#11213,#11214);
#9601=AXIS2_PLACEMENT_3D('',#14257,#11218,#11219);
#9602=AXIS2_PLACEMENT_3D('',#14261,#11222,#11223);
#9603=AXIS2_PLACEMENT_3D('',#14265,#11226,#11227);
#9604=AXIS2_PLACEMENT_3D('',#14269,#11230,#11231);
#9605=AXIS2_PLACEMENT_3D('',#14273,#11234,#11235);
#9606=AXIS2_PLACEMENT_3D('',#14277,#11238,#11239);
#9607=AXIS2_PLACEMENT_3D('',#14279,#11241,#11242);
#9608=AXIS2_PLACEMENT_3D('',#14283,#11245,#11246);
#9609=AXIS2_PLACEMENT_3D('',#14287,#11249,#11250);
#9610=AXIS2_PLACEMENT_3D('',#14291,#11253,#11254);
#9611=AXIS2_PLACEMENT_3D('',#14295,#11257,#11258);
#9612=AXIS2_PLACEMENT_3D('',#14299,#11261,#11262);
#9613=AXIS2_PLACEMENT_3D('',#14303,#11265,#11266);
#9614=AXIS2_PLACEMENT_3D('',#14307,#11269,#11270);
#9615=AXIS2_PLACEMENT_3D('',#14311,#11273,#11274);
#9616=AXIS2_PLACEMENT_3D('',#14315,#11277,#11278);
#9617=AXIS2_PLACEMENT_3D('',#14317,#11280,#11281);
#9618=AXIS2_PLACEMENT_3D('',#14323,#11285,#11286);
#9619=AXIS2_PLACEMENT_3D('',#14327,#11289,#11290);
#9620=AXIS2_PLACEMENT_3D('',#14331,#11293,#11294);
#9621=AXIS2_PLACEMENT_3D('',#14335,#11297,#11298);
#9622=AXIS2_PLACEMENT_3D('',#14339,#11301,#11302);
#9623=AXIS2_PLACEMENT_3D('',#14343,#11305,#11306);
#9624=AXIS2_PLACEMENT_3D('',#14346,#11309,#11310);
#9625=AXIS2_PLACEMENT_3D('',#14347,#11311,#11312);
#9626=AXIS2_PLACEMENT_3D('',#14349,#11314,#11315);
#9627=AXIS2_PLACEMENT_3D('',#14351,#11317,#11318);
#9628=AXIS2_PLACEMENT_3D('',#14353,#11320,#11321);
#9629=AXIS2_PLACEMENT_3D('',#14355,#11323,#11324);
#9630=AXIS2_PLACEMENT_3D('',#14357,#11326,#11327);
#9631=AXIS2_PLACEMENT_3D('',#14359,#11329,#11330);
#9632=AXIS2_PLACEMENT_3D('',#14361,#11332,#11333);
#9633=AXIS2_PLACEMENT_3D('',#14365,#11336,#11337);
#9634=AXIS2_PLACEMENT_3D('',#14369,#11340,#11341);
#9635=AXIS2_PLACEMENT_3D('',#14373,#11344,#11345);
#9636=AXIS2_PLACEMENT_3D('',#14377,#11348,#11349);
#9637=AXIS2_PLACEMENT_3D('',#14381,#11352,#11353);
#9638=AXIS2_PLACEMENT_3D('',#14387,#11357,#11358);
#9639=AXIS2_PLACEMENT_3D('',#14391,#11361,#11362);
#9640=AXIS2_PLACEMENT_3D('',#14395,#11365,#11366);
#9641=AXIS2_PLACEMENT_3D('',#14397,#11368,#11369);
#9642=AXIS2_PLACEMENT_3D('',#14399,#11371,#11372);
#9643=AXIS2_PLACEMENT_3D('',#14401,#11374,#11375);
#9644=AXIS2_PLACEMENT_3D('',#14403,#11377,#11378);
#9645=AXIS2_PLACEMENT_3D('',#14406,#11380,#11381);
#9646=AXIS2_PLACEMENT_3D('',#14408,#11382,#11383);
#9647=AXIS2_PLACEMENT_3D('',#14410,#11384,#11385);
#9648=AXIS2_PLACEMENT_3D('',#14411,#11386,#11387);
#9649=AXIS2_PLACEMENT_3D('',#14413,#11389,#11390);
#9650=AXIS2_PLACEMENT_3D('',#14415,#11392,#11393);
#9651=AXIS2_PLACEMENT_3D('',#14417,#11395,#11396);
#9652=AXIS2_PLACEMENT_3D('',#14419,#11398,#11399);
#9653=AXIS2_PLACEMENT_3D('',#14421,#11401,#11402);
#9654=AXIS2_PLACEMENT_3D('',#14423,#11404,#11405);
#9655=AXIS2_PLACEMENT_3D('',#14425,#11407,#11408);
#9656=AXIS2_PLACEMENT_3D('',#14426,#11409,#11410);
#9657=AXIS2_PLACEMENT_3D('',#14427,#11411,#11412);
#9658=AXIS2_PLACEMENT_3D('',#14428,#11413,#11414);
#9659=AXIS2_PLACEMENT_3D('',#14429,#11415,#11416);
#9660=AXIS2_PLACEMENT_3D('',#14430,#11417,#11418);
#9661=AXIS2_PLACEMENT_3D('',#14432,#11420,#11421);
#9662=AXIS2_PLACEMENT_3D('',#14434,#11423,#11424);
#9663=AXIS2_PLACEMENT_3D('',#14436,#11426,#11427);
#9664=AXIS2_PLACEMENT_3D('',#14437,#11428,#11429);
#9665=AXIS2_PLACEMENT_3D('',#14438,#11430,#11431);
#9666=AXIS2_PLACEMENT_3D('',#14440,#11432,#11433);
#9667=AXIS2_PLACEMENT_3D('',#14441,#11434,#11435);
#9668=AXIS2_PLACEMENT_3D('',#14443,#11436,#11437);
#9669=AXIS2_PLACEMENT_3D('',#14445,#11439,#11440);
#9670=AXIS2_PLACEMENT_3D('',#14447,#11441,#11442);
#9671=AXIS2_PLACEMENT_3D('',#14449,#11444,#11445);
#9672=AXIS2_PLACEMENT_3D('',#14451,#11446,#11447);
#9673=AXIS2_PLACEMENT_3D('',#14453,#11449,#11450);
#9674=AXIS2_PLACEMENT_3D('',#14454,#11451,#11452);
#9675=AXIS2_PLACEMENT_3D('',#14455,#11453,#11454);
#9676=AXIS2_PLACEMENT_3D('',#14457,#11455,#11456);
#9677=AXIS2_PLACEMENT_3D('',#14461,#11458,#11459);
#9678=AXIS2_PLACEMENT_3D('',#14462,#11460,#11461);
#9679=AXIS2_PLACEMENT_3D('',#14463,#11462,#11463);
#9680=AXIS2_PLACEMENT_3D('',#14466,#11465,#11466);
#9681=AXIS2_PLACEMENT_3D('',#14467,#11467,#11468);
#9682=AXIS2_PLACEMENT_3D('',#14468,#11469,#11470);
#9683=AXIS2_PLACEMENT_3D('',#14481,#11473,#11474);
#9684=AXIS2_PLACEMENT_3D('',#14482,#11475,#11476);
#9685=AXIS2_PLACEMENT_3D('',#14484,#11477,#11478);
#9686=AXIS2_PLACEMENT_3D('',#14485,#11479,#11480);
#9687=AXIS2_PLACEMENT_3D('',#14486,#11481,#11482);
#9688=AXIS2_PLACEMENT_3D('',#14487,#11483,#11484);
#9689=AXIS2_PLACEMENT_3D('',#14490,#11485,#11486);
#9690=AXIS2_PLACEMENT_3D('',#14492,#11488,#11489);
#9691=AXIS2_PLACEMENT_3D('',#14495,#11492,#11493);
#9692=AXIS2_PLACEMENT_3D('',#14497,#11494,#11495);
#9693=AXIS2_PLACEMENT_3D('',#14499,#11497,#11498);
#9694=AXIS2_PLACEMENT_3D('',#14501,#11499,#11500);
#9695=AXIS2_PLACEMENT_3D('',#14502,#11501,#11502);
#9696=AXIS2_PLACEMENT_3D('',#14504,#11504,#11505);
#9697=AXIS2_PLACEMENT_3D('',#14505,#11506,#11507);
#9698=AXIS2_PLACEMENT_3D('',#14508,#11508,#11509);
#9699=AXIS2_PLACEMENT_3D('',#14509,#11510,#11511);
#9700=AXIS2_PLACEMENT_3D('',#14512,#11513,#11514);
#9701=AXIS2_PLACEMENT_3D('',#14513,#11515,#11516);
#9702=AXIS2_PLACEMENT_3D('',#14514,#11517,#11518);
#9703=AXIS2_PLACEMENT_3D('',#14516,#11519,#11520);
#9704=AXIS2_PLACEMENT_3D('',#14518,#11522,#11523);
#9705=AXIS2_PLACEMENT_3D('',#14520,#11524,#11525);
#9706=AXIS2_PLACEMENT_3D('',#14522,#11527,#11528);
#9707=AXIS2_PLACEMENT_3D('',#14524,#11529,#11530);
#9708=AXIS2_PLACEMENT_3D('',#14525,#11531,#11532);
#9709=AXIS2_PLACEMENT_3D('',#14527,#11533,#11534);
#9710=AXIS2_PLACEMENT_3D('',#14529,#11536,#11537);
#9711=AXIS2_PLACEMENT_3D('',#14531,#11538,#11539);
#9712=AXIS2_PLACEMENT_3D('',#14533,#11541,#11542);
#9713=AXIS2_PLACEMENT_3D('',#14534,#11543,#11544);
#9714=AXIS2_PLACEMENT_3D('',#14535,#11545,#11546);
#9715=AXIS2_PLACEMENT_3D('',#14538,#11547,#11548);
#9716=AXIS2_PLACEMENT_3D('',#14539,#11549,#11550);
#9717=AXIS2_PLACEMENT_3D('',#14542,#11552,#11553);
#9718=AXIS2_PLACEMENT_3D('',#14543,#11554,#11555);
#9719=AXIS2_PLACEMENT_3D('',#14545,#11556,#11557);
#9720=AXIS2_PLACEMENT_3D('',#14546,#11558,#11559);
#9721=AXIS2_PLACEMENT_3D('',#14548,#11560,#11561);
#9722=AXIS2_PLACEMENT_3D('',#14550,#11563,#11564);
#9723=AXIS2_PLACEMENT_3D('',#14552,#11565,#11566);
#9724=AXIS2_PLACEMENT_3D('',#14554,#11568,#11569);
#9725=AXIS2_PLACEMENT_3D('',#14556,#11570,#11571);
#9726=AXIS2_PLACEMENT_3D('',#14557,#11572,#11573);
#9727=AXIS2_PLACEMENT_3D('',#14559,#11574,#11575);
#9728=AXIS2_PLACEMENT_3D('',#14561,#11577,#11578);
#9729=AXIS2_PLACEMENT_3D('',#14562,#11579,#11580);
#9730=AXIS2_PLACEMENT_3D('',#14563,#11581,#11582);
#9731=AXIS2_PLACEMENT_3D('',#14568,#11584,#11585);
#9732=AXIS2_PLACEMENT_3D('',#14571,#11587,#11588);
#9733=AXIS2_PLACEMENT_3D('',#14572,#11589,#11590);
#9734=AXIS2_PLACEMENT_3D('',#14576,#11592,#11593);
#9735=AXIS2_PLACEMENT_3D('',#14578,#11595,#11596);
#9736=AXIS2_PLACEMENT_3D('',#14582,#11598,#11599);
#9737=AXIS2_PLACEMENT_3D('',#14585,#11601,#11602);
#9738=AXIS2_PLACEMENT_3D('',#14586,#11603,#11604);
#9739=AXIS2_PLACEMENT_3D('',#14590,#11606,#11607);
#9740=AXIS2_PLACEMENT_3D('',#14592,#11609,#11610);
#9741=AXIS2_PLACEMENT_3D('',#14594,#11612,#11613);
#9742=AXIS2_PLACEMENT_3D('',#14599,#11615,#11616);
#9743=AXIS2_PLACEMENT_3D('',#14602,#11618,#11619);
#9744=AXIS2_PLACEMENT_3D('',#14603,#11620,#11621);
#9745=AXIS2_PLACEMENT_3D('',#14609,#11625,#11626);
#9746=AXIS2_PLACEMENT_3D('',#14613,#11628,#11629);
#9747=AXIS2_PLACEMENT_3D('',#14616,#11631,#11632);
#9748=AXIS2_PLACEMENT_3D('',#14617,#11633,#11634);
#9749=AXIS2_PLACEMENT_3D('',#14620,#11636,#11637);
#9750=AXIS2_PLACEMENT_3D('',#14621,#11638,#11639);
#9751=AXIS2_PLACEMENT_3D('',#14623,#11640,#11641);
#9752=AXIS2_PLACEMENT_3D('',#14748,#11644,#11645);
#9753=AXIS2_PLACEMENT_3D('',#14788,#11647,#11648);
#9754=AXIS2_PLACEMENT_3D('',#14790,#11649,#11650);
#9755=AXIS2_PLACEMENT_3D('',#14792,#11651,#11652);
#9756=AXIS2_PLACEMENT_3D('',#14794,#11653,#11654);
#9757=AXIS2_PLACEMENT_3D('',#14796,#11655,#11656);
#9758=AXIS2_PLACEMENT_3D('',#14799,#11658,#11659);
#9759=AXIS2_PLACEMENT_3D('',#14801,#11660,#11661);
#9760=AXIS2_PLACEMENT_3D('',#14802,#11662,#11663);
#9761=AXIS2_PLACEMENT_3D('',#14804,#11664,#11665);
#9762=AXIS2_PLACEMENT_3D('',#14806,#11666,#11667);
#9763=AXIS2_PLACEMENT_3D('',#14807,#11668,#11669);
#9764=AXIS2_PLACEMENT_3D('',#14808,#11670,#11671);
#9765=AXIS2_PLACEMENT_3D('',#14810,#11672,#11673);
#9766=AXIS2_PLACEMENT_3D('',#14811,#11674,#11675);
#9767=AXIS2_PLACEMENT_3D('',#14824,#11678,#11679);
#9768=AXIS2_PLACEMENT_3D('',#14834,#11681,#11682);
#9769=AXIS2_PLACEMENT_3D('',#14843,#11687,#11688);
#9770=AXIS2_PLACEMENT_3D('',#14849,#11692,#11693);
#9771=AXIS2_PLACEMENT_3D('',#14858,#11698,#11699);
#9772=AXIS2_PLACEMENT_3D('',#14864,#11703,#11704);
#9773=AXIS2_PLACEMENT_3D('',#14873,#11709,#11710);
#9774=AXIS2_PLACEMENT_3D('',#14879,#11714,#11715);
#9775=AXIS2_PLACEMENT_3D('',#14888,#11720,#11721);
#9776=AXIS2_PLACEMENT_3D('',#14894,#11725,#11726);
#9777=AXIS2_PLACEMENT_3D('',#14907,#11729,#11730);
#9778=AXIS2_PLACEMENT_3D('',#14917,#11732,#11733);
#9779=AXIS2_PLACEMENT_3D('',#14930,#11736,#11737);
#9780=AXIS2_PLACEMENT_3D('',#14940,#11739,#11740);
#9781=AXIS2_PLACEMENT_3D('',#14949,#11745,#11746);
#9782=AXIS2_PLACEMENT_3D('',#14955,#11750,#11751);
#9783=AXIS2_PLACEMENT_3D('',#14964,#11756,#11757);
#9784=AXIS2_PLACEMENT_3D('',#14970,#11761,#11762);
#9785=AXIS2_PLACEMENT_3D('',#14983,#11765,#11766);
#9786=AXIS2_PLACEMENT_3D('',#14993,#11768,#11769);
#9787=AXIS2_PLACEMENT_3D('',#15002,#11774,#11775);
#9788=AXIS2_PLACEMENT_3D('',#15008,#11779,#11780);
#9789=AXIS2_PLACEMENT_3D('',#15021,#11783,#11784);
#9790=AXIS2_PLACEMENT_3D('',#15031,#11786,#11787);
#9791=AXIS2_PLACEMENT_3D('',#15044,#11790,#11791);
#9792=AXIS2_PLACEMENT_3D('',#15054,#11793,#11794);
#9793=AXIS2_PLACEMENT_3D('',#15056,#11795,#11796);
#9794=AXIS2_PLACEMENT_3D('',#15060,#11798,#11799);
#9795=AXIS2_PLACEMENT_3D('',#15062,#11801,#11802);
#9796=AXIS2_PLACEMENT_3D('',#15063,#11803,#11804);
#9797=AXIS2_PLACEMENT_3D('',#15064,#11805,#11806);
#9798=AXIS2_PLACEMENT_3D('',#15077,#11817,#11818);
#9799=AXIS2_PLACEMENT_3D('',#15078,#11819,#11820);
#9800=AXIS2_PLACEMENT_3D('',#15079,#11821,#11822);
#9801=AXIS2_PLACEMENT_3D('',#15080,#11823,#11824);
#9802=AXIS2_PLACEMENT_3D('',#15083,#11826,#11827);
#9803=AXIS2_PLACEMENT_3D('',#15084,#11828,#11829);
#9804=AXIS2_PLACEMENT_3D('',#15085,#11830,#11831);
#9805=AXIS2_PLACEMENT_3D('',#15087,#11833,#11834);
#9806=AXIS2_PLACEMENT_3D('',#15089,#11836,#11837);
#9807=AXIS2_PLACEMENT_3D('',#15090,#11838,#11839);
#9808=AXIS2_PLACEMENT_3D('',#15091,#11840,#11841);
#9809=AXIS2_PLACEMENT_3D('',#15092,#11842,#11843);
#9810=AXIS2_PLACEMENT_3D('',#15093,#11844,#11845);
#9811=AXIS2_PLACEMENT_3D('',#15095,#11846,#11847);
#9812=AXIS2_PLACEMENT_3D('',#15097,#11849,#11850);
#9813=AXIS2_PLACEMENT_3D('',#15099,#11852,#11853);
#9814=AXIS2_PLACEMENT_3D('',#15101,#11855,#11856);
#9815=AXIS2_PLACEMENT_3D('',#15103,#11858,#11859);
#9816=AXIS2_PLACEMENT_3D('',#15105,#11861,#11862);
#9817=AXIS2_PLACEMENT_3D('',#15108,#11864,#11865);
#9818=AXIS2_PLACEMENT_3D('',#15109,#11866,#11867);
#9819=AXIS2_PLACEMENT_3D('',#15110,#11868,#11869);
#9820=AXIS2_PLACEMENT_3D('',#15113,#11872,#11873);
#9821=AXIS2_PLACEMENT_3D('',#15119,#11878,#11879);
#9822=AXIS2_PLACEMENT_3D('',#15122,#11882,#11883);
#9823=AXIS2_PLACEMENT_3D('',#15128,#11888,#11889);
#9824=AXIS2_PLACEMENT_3D('',#15130,#11891,#11892);
#9825=AXIS2_PLACEMENT_3D('',#15131,#11893,#11894);
#9826=AXIS2_PLACEMENT_3D('',#15134,#11896,#11897);
#9827=AXIS2_PLACEMENT_3D('',#15135,#11898,#11899);
#9828=AXIS2_PLACEMENT_3D('',#15136,#11900,#11901);
#9829=AXIS2_PLACEMENT_3D('',#15138,#11902,#11903);
#9830=AXIS2_PLACEMENT_3D('',#15140,#11905,#11906);
#9831=AXIS2_PLACEMENT_3D('',#15142,#11908,#11909);
#9832=AXIS2_PLACEMENT_3D('',#15145,#11912,#11913);
#9833=AXIS2_PLACEMENT_3D('',#15146,#11914,#11915);
#9834=AXIS2_PLACEMENT_3D('',#15148,#11917,#11918);
#9835=AXIS2_PLACEMENT_3D('',#15149,#11919,#11920);
#9836=AXIS2_PLACEMENT_3D('',#15151,#11922,#11923);
#9837=AXIS2_PLACEMENT_3D('',#15152,#11924,#11925);
#9838=AXIS2_PLACEMENT_3D('',#15153,#11926,#11927);
#9839=AXIS2_PLACEMENT_3D('',#15155,#11929,#11930);
#9840=AXIS2_PLACEMENT_3D('',#15156,#11931,#11932);
#9841=AXIS2_PLACEMENT_3D('',#15157,#11933,#11934);
#9842=AXIS2_PLACEMENT_3D('',#15158,#11935,#11936);
#9843=AXIS2_PLACEMENT_3D('',#15161,#11938,#11939);
#9844=AXIS2_PLACEMENT_3D('',#15162,#11940,#11941);
#9845=AXIS2_PLACEMENT_3D('',#15164,#11942,#11943);
#9846=AXIS2_PLACEMENT_3D('',#15165,#11944,#11945);
#9847=AXIS2_PLACEMENT_3D('',#15167,#11947,#11948);
#9848=AXIS2_PLACEMENT_3D('',#15168,#11949,#11950);
#9849=AXIS2_PLACEMENT_3D('',#15184,#11952,#11953);
#9850=AXIS2_PLACEMENT_3D('',#15192,#11954,#11955);
#9851=AXIS2_PLACEMENT_3D('',#15240,#11957,#11958);
#9852=AXIS2_PLACEMENT_3D('',#15288,#11960,#11961);
#9853=AXIS2_PLACEMENT_3D('',#15342,#11963,#11964);
#9854=AXIS2_PLACEMENT_3D('',#15390,#11966,#11967);
#9855=AXIS2_PLACEMENT_3D('',#15399,#11969,#11970);
#9856=AXIS2_PLACEMENT_3D('',#15400,#11971,#11972);
#9857=AXIS2_PLACEMENT_3D('',#15415,#11974,#11975);
#9858=AXIS2_PLACEMENT_3D('',#15425,#11976,#11977);
#9859=AXIS2_PLACEMENT_3D('',#15450,#11979,#11980);
#9860=AXIS2_PLACEMENT_3D('',#15475,#11982,#11983);
#9861=AXIS2_PLACEMENT_3D('',#15499,#11985,#11986);
#9862=AXIS2_PLACEMENT_3D('',#15590,#11987,#11988);
#9863=AXIS2_PLACEMENT_3D('',#15592,#11989,#11990);
#9864=AXIS2_PLACEMENT_3D('',#15932,#11991,#11992);
#9865=AXIS2_PLACEMENT_3D('',#15934,#11993,#11994);
#9866=AXIS2_PLACEMENT_3D('',#15935,#11995,#11996);
#9867=AXIS2_PLACEMENT_3D('',#16025,#11997,#11998);
#9868=AXIS2_PLACEMENT_3D('',#16026,#11999,#12000);
#9869=AXIS2_PLACEMENT_3D('',#16185,#12001,#12002);
#9870=AXIS2_PLACEMENT_3D('',#16194,#12007,#12008);
#9871=AXIS2_PLACEMENT_3D('',#16200,#12012,#12013);
#9872=AXIS2_PLACEMENT_3D('',#16206,#12017,#12018);
#9873=AXIS2_PLACEMENT_3D('',#16212,#12022,#12023);
#9874=AXIS2_PLACEMENT_3D('',#16218,#12027,#12028);
#9875=AXIS2_PLACEMENT_3D('',#16221,#12031,#12032);
#9876=AXIS2_PLACEMENT_3D('',#16222,#12033,#12034);
#9877=AXIS2_PLACEMENT_3D('',#16224,#12035,#12036);
#9878=AXIS2_PLACEMENT_3D('',#16225,#12037,#12038);
#9879=AXIS2_PLACEMENT_3D('',#16227,#12040,#12041);
#9880=AXIS2_PLACEMENT_3D('',#16228,#12042,#12043);
#9881=AXIS2_PLACEMENT_3D('',#16229,#12044,#12045);
#9882=AXIS2_PLACEMENT_3D('',#16231,#12046,#12047);
#9883=AXIS2_PLACEMENT_3D('',#16233,#12049,#12050);
#9884=AXIS2_PLACEMENT_3D('',#16234,#12051,#12052);
#9885=AXIS2_PLACEMENT_3D('',#16235,#12053,#12054);
#9886=AXIS2_PLACEMENT_3D('',#16251,#12056,#12057);
#9887=AXIS2_PLACEMENT_3D('',#16259,#12058,#12059);
#9888=AXIS2_PLACEMENT_3D('',#16307,#12061,#12062);
#9889=AXIS2_PLACEMENT_3D('',#16355,#12064,#12065);
#9890=AXIS2_PLACEMENT_3D('',#16409,#12067,#12068);
#9891=AXIS2_PLACEMENT_3D('',#16457,#12070,#12071);
#9892=AXIS2_PLACEMENT_3D('',#16505,#12073,#12074);
#9893=AXIS2_PLACEMENT_3D('',#16559,#12076,#12077);
#9894=AXIS2_PLACEMENT_3D('',#16607,#12079,#12080);
#9895=AXIS2_PLACEMENT_3D('',#16655,#12082,#12083);
#9896=AXIS2_PLACEMENT_3D('',#16709,#12085,#12086);
#9897=AXIS2_PLACEMENT_3D('',#16757,#12088,#12089);
#9898=AXIS2_PLACEMENT_3D('',#16811,#12091,#12092);
#9899=AXIS2_PLACEMENT_3D('',#16823,#12094,#12095);
#9900=AXIS2_PLACEMENT_3D('',#16829,#12096,#12097);
#9901=AXIS2_PLACEMENT_3D('',#16854,#12099,#12100);
#9902=AXIS2_PLACEMENT_3D('',#16879,#12102,#12103);
#9903=AXIS2_PLACEMENT_3D('',#16904,#12105,#12106);
#9904=AXIS2_PLACEMENT_3D('',#16929,#12108,#12109);
#9905=AXIS2_PLACEMENT_3D('',#16953,#12111,#12112);
#9906=AXIS2_PLACEMENT_3D('',#16978,#12114,#12115);
#9907=AXIS2_PLACEMENT_3D('',#17003,#12117,#12118);
#9908=AXIS2_PLACEMENT_3D('',#17027,#12120,#12121);
#9909=AXIS2_PLACEMENT_3D('',#17052,#12123,#12124);
#9910=AXIS2_PLACEMENT_3D('',#17077,#12126,#12127);
#9911=AXIS2_PLACEMENT_3D('',#17101,#12129,#12130);
#9912=AXIS2_PLACEMENT_3D('',#17189,#12131,#12132);
#9913=AXIS2_PLACEMENT_3D('',#17191,#12133,#12134);
#9914=AXIS2_PLACEMENT_3D('',#17716,#12135,#12136);
#9915=AXIS2_PLACEMENT_3D('',#17718,#12137,#12138);
#9916=AXIS2_PLACEMENT_3D('',#17719,#12139,#12140);
#9917=AXIS2_PLACEMENT_3D('',#17803,#12141,#12142);
#9918=AXIS2_PLACEMENT_3D('',#17804,#12143,#12144);
#9919=AXIS2_PLACEMENT_3D('',#18157,#12145,#12146);
#9920=AXIS2_PLACEMENT_3D('',#18161,#12148,#12149);
#9921=AXIS2_PLACEMENT_3D('',#18162,#12150,#12151);
#9922=AXIS2_PLACEMENT_3D('',#18171,#12156,#12157);
#9923=AXIS2_PLACEMENT_3D('',#18177,#12161,#12162);
#9924=AXIS2_PLACEMENT_3D('',#18183,#12166,#12167);
#9925=AXIS2_PLACEMENT_3D('',#18189,#12171,#12172);
#9926=AXIS2_PLACEMENT_3D('',#18195,#12176,#12177);
#9927=AXIS2_PLACEMENT_3D('',#18198,#12180,#12181);
#9928=AXIS2_PLACEMENT_3D('',#18199,#12182,#12183);
#9929=AXIS2_PLACEMENT_3D('',#18201,#12184,#12185);
#9930=AXIS2_PLACEMENT_3D('',#18202,#12186,#12187);
#9931=AXIS2_PLACEMENT_3D('',#18204,#12189,#12190);
#9932=AXIS2_PLACEMENT_3D('',#18205,#12191,#12192);
#9933=AXIS2_PLACEMENT_3D('',#18206,#12193,#12194);
#9934=AXIS2_PLACEMENT_3D('',#18208,#12195,#12196);
#9935=AXIS2_PLACEMENT_3D('',#18210,#12198,#12199);
#9936=AXIS2_PLACEMENT_3D('',#18211,#12200,#12201);
#9937=AXIS2_PLACEMENT_3D('',#18212,#12202,#12203);
#9938=AXIS2_PLACEMENT_3D('',#18214,#12204,#12205);
#9939=AXIS2_PLACEMENT_3D('',#18215,#12206,#12207);
#9940=AXIS2_PLACEMENT_3D('',#18217,#12208,#12209);
#9941=AXIS2_PLACEMENT_3D('',#18219,#12211,#12212);
#9942=AXIS2_PLACEMENT_3D('',#18221,#12213,#12214);
#9943=AXIS2_PLACEMENT_3D('',#18223,#12216,#12217);
#9944=AXIS2_PLACEMENT_3D('',#18225,#12218,#12219);
#9945=AXIS2_PLACEMENT_3D('',#18227,#12221,#12222);
#9946=AXIS2_PLACEMENT_3D('',#18228,#12223,#12224);
#9947=AXIS2_PLACEMENT_3D('',#18229,#12225,#12226);
#9948=AXIS2_PLACEMENT_3D('',#18230,#12227,#12228);
#9949=AXIS2_PLACEMENT_3D('',#18231,#12229,#12230);
#9950=AXIS2_PLACEMENT_3D('',#18232,#12231,#12232);
#9951=AXIS2_PLACEMENT_3D('',#18233,#12233,#12234);
#9952=AXIS2_PLACEMENT_3D('',#18234,#12235,#12236);
#9953=AXIS2_PLACEMENT_3D('',#18235,#12237,#12238);
#9954=AXIS2_PLACEMENT_3D('',#18236,#12239,#12240);
#9955=AXIS2_PLACEMENT_3D('',#18237,#12241,#12242);
#9956=AXIS2_PLACEMENT_3D('',#18238,#12243,#12244);
#9957=AXIS2_PLACEMENT_3D('',#18239,#12245,#12246);
#9958=AXIS2_PLACEMENT_3D('',#18240,#12247,#12248);
#9959=AXIS2_PLACEMENT_3D('',#18241,#12249,#12250);
#9960=AXIS2_PLACEMENT_3D('',#18242,#12251,#12252);
#9961=AXIS2_PLACEMENT_3D('',#18243,#12253,#12254);
#9962=AXIS2_PLACEMENT_3D('',#18244,#12255,#12256);
#9963=AXIS2_PLACEMENT_3D('',#18245,#12257,#12258);
#9964=AXIS2_PLACEMENT_3D('',#18246,#12259,#12260);
#9965=AXIS2_PLACEMENT_3D('',#18247,#12261,#12262);
#9966=AXIS2_PLACEMENT_3D('',#18248,#12263,#12264);
#9967=AXIS2_PLACEMENT_3D('',#18249,#12265,#12266);
#9968=AXIS2_PLACEMENT_3D('',#18250,#12267,#12268);
#9969=AXIS2_PLACEMENT_3D('',#18251,#12269,#12270);
#9970=DIRECTION('axis',(0.,0.,1.));
#9971=DIRECTION('refdir',(1.,0.,0.));
#9972=DIRECTION('axis',(0.,0.,1.));
#9973=DIRECTION('refdir',(1.,0.,0.));
#9974=DIRECTION('center_axis',(0.57735026918962,0.577350269189628,-0.57735026918963));
#9975=DIRECTION('ref_axis',(-0.707106781186554,0.,-0.707106781186541));
#9976=DIRECTION('',(0.707106781186554,0.,0.707106781186541));
#9977=DIRECTION('',(0.,-0.707106781186549,-0.707106781186546));
#9978=DIRECTION('',(-0.707106781186552,0.707106781186543,0.));
#9979=DIRECTION('center_axis',(-0.577350269189622,0.577350269189627,-0.577350269189629));
#9980=DIRECTION('ref_axis',(-0.707106781186552,0.,0.707106781186543));
#9981=DIRECTION('',(0.,0.707106781186549,0.707106781186546));
#9982=DIRECTION('',(0.707106781186552,0.,-0.707106781186543));
#9983=DIRECTION('',(-0.707106781186547,-0.707106781186548,-6.2803698347351E-15));
#9984=DIRECTION('center_axis',(0.57735026918962,-0.577350269189628,-0.57735026918963));
#9985=DIRECTION('ref_axis',(-0.707106781186554,0.,-0.707106781186541));
#9986=DIRECTION('',(0.707106781186552,0.707106781186543,0.));
#9987=DIRECTION('',(0.,-0.707106781186549,0.707106781186546));
#9988=DIRECTION('',(-0.707106781186554,0.,-0.707106781186541));
#9989=DIRECTION('center_axis',(-0.577350269189622,-0.577350269189627,-0.577350269189629));
#9990=DIRECTION('ref_axis',(-0.707106781186552,0.,0.707106781186543));
#9991=DIRECTION('',(0.,0.707106781186549,-0.707106781186546));
#9992=DIRECTION('',(0.707106781186547,-0.707106781186548,6.2803698347351E-15));
#9993=DIRECTION('',(-0.707106781186552,0.,0.707106781186543));
#9994=DIRECTION('center_axis',(-0.707106781186548,-0.707106781186547,0.));
#9995=DIRECTION('ref_axis',(0.,0.,1.));
#9996=DIRECTION('center_axis',(0.707106781186548,0.707106781186547,0.));
#9997=DIRECTION('ref_axis',(-0.707106781186547,0.707106781186548,0.));
#9998=DIRECTION('',(0.,0.,-1.));
#9999=DIRECTION('',(0.,0.,1.));
#10000=DIRECTION('center_axis',(-0.707106781186543,0.,-0.707106781186552));
#10001=DIRECTION('ref_axis',(-0.707106781186552,0.,0.707106781186543));
#10002=DIRECTION('',(0.,-1.,0.));
#10003=DIRECTION('',(0.,1.,0.));
#10004=DIRECTION('center_axis',(0.,-0.707106781186546,-0.707106781186549));
#10005=DIRECTION('ref_axis',(-1.,0.,0.));
#10006=DIRECTION('',(-1.,0.,0.));
#10007=DIRECTION('',(1.,0.,0.));
#10008=DIRECTION('center_axis',(0.707106781186541,0.,-0.707106781186554));
#10009=DIRECTION('ref_axis',(-0.707106781186554,0.,-0.707106781186541));
#10010=DIRECTION('',(0.,-1.,0.));
#10011=DIRECTION('',(0.,1.,0.));
#10012=DIRECTION('center_axis',(0.707106781186543,-0.707106781186552,0.));
#10013=DIRECTION('ref_axis',(0.,0.,-1.));
#10014=DIRECTION('center_axis',(-0.707106781186543,0.707106781186552,0.));
#10015=DIRECTION('ref_axis',(0.707106781186552,0.707106781186543,0.));
#10016=DIRECTION('',(0.,0.,-1.));
#10017=DIRECTION('',(0.,0.,1.));
#10018=DIRECTION('center_axis',(-0.707106781186548,0.707106781186547,0.));
#10019=DIRECTION('ref_axis',(0.,0.,1.));
#10020=DIRECTION('center_axis',(0.707106781186548,-0.707106781186547,0.));
#10021=DIRECTION('ref_axis',(0.707106781186547,0.707106781186548,0.));
#10022=DIRECTION('',(0.,0.,-1.));
#10023=DIRECTION('',(0.,0.,1.));
#10024=DIRECTION('center_axis',(0.,0.707106781186546,-0.707106781186549));
#10025=DIRECTION('ref_axis',(-1.,0.,0.));
#10026=DIRECTION('',(-1.,0.,0.));
#10027=DIRECTION('',(1.,0.,0.));
#10028=DIRECTION('center_axis',(0.707106781186543,0.707106781186552,0.));
#10029=DIRECTION('ref_axis',(0.,0.,-1.));
#10030=DIRECTION('center_axis',(-0.707106781186543,-0.707106781186552,0.));
#10031=DIRECTION('ref_axis',(-0.707106781186552,0.707106781186543,0.));
#10032=DIRECTION('',(0.,0.,-1.));
#10033=DIRECTION('',(0.,0.,1.));
#10034=DIRECTION('center_axis',(0.,-1.,0.));
#10035=DIRECTION('ref_axis',(0.,0.,-1.));
#10036=DIRECTION('',(-1.,0.,0.));
#10037=DIRECTION('center_axis',(0.,1.,0.));
#10038=DIRECTION('ref_axis',(1.,0.,0.));
#10039=DIRECTION('center_axis',(0.,1.,0.));
#10040=DIRECTION('ref_axis',(1.,0.,0.));
#10041=DIRECTION('center_axis',(0.,1.,0.));
#10042=DIRECTION('ref_axis',(1.,0.,0.));
#10043=DIRECTION('center_axis',(1.,0.,0.));
#10044=DIRECTION('ref_axis',(0.,0.,-1.));
#10045=DIRECTION('center_axis',(-1.,0.,0.));
#10046=DIRECTION('ref_axis',(0.,0.,-1.));
#10047=DIRECTION('center_axis',(0.,0.,-1.));
#10048=DIRECTION('ref_axis',(0.,1.,0.));
#10049=DIRECTION('center_axis',(0.,-1.,0.));
#10050=DIRECTION('ref_axis',(1.,0.,0.));
#10051=DIRECTION('center_axis',(0.,-1.,0.));
#10052=DIRECTION('ref_axis',(1.,0.,0.));
#10053=DIRECTION('',(0.,-1.,0.));
#10054=DIRECTION('center_axis',(0.,-1.,0.));
#10055=DIRECTION('ref_axis',(1.,0.,0.));
#10056=DIRECTION('center_axis',(0.,-1.,0.));
#10057=DIRECTION('ref_axis',(1.,0.,0.));
#10058=DIRECTION('',(0.,-1.,0.));
#10059=DIRECTION('center_axis',(0.,-1.,0.));
#10060=DIRECTION('ref_axis',(1.,0.,0.));
#10061=DIRECTION('center_axis',(0.,-1.,0.));
#10062=DIRECTION('ref_axis',(1.,0.,0.));
#10063=DIRECTION('',(0.,-1.,0.));
#10064=DIRECTION('center_axis',(1.,0.,0.));
#10065=DIRECTION('ref_axis',(0.,0.,-1.));
#10066=DIRECTION('',(1.,0.,0.));
#10067=DIRECTION('center_axis',(1.,0.,0.));
#10068=DIRECTION('ref_axis',(0.,0.,-1.));
#10069=DIRECTION('center_axis',(1.,0.,0.));
#10070=DIRECTION('ref_axis',(0.,0.,-1.));
#10071=DIRECTION('center_axis',(0.,1.,0.));
#10072=DIRECTION('ref_axis',(0.,0.,1.));
#10073=DIRECTION('axis',(0.,0.,1.));
#10074=DIRECTION('refdir',(1.,0.,0.));
#10075=DIRECTION('center_axis',(0.577350269189623,-0.577350269189631,0.577350269189623));
#10076=DIRECTION('ref_axis',(0.707106781186548,0.,-0.707106781186548));
#10077=DIRECTION('',(0.707106781186547,0.,-0.707106781186547));
#10078=DIRECTION('',(0.,0.707106781186543,0.707106781186552));
#10079=DIRECTION('',(-0.707106781186552,-0.707106781186543,0.));
#10080=DIRECTION('center_axis',(-0.577350269189642,-0.577350269189621,0.577350269189614));
#10081=DIRECTION('ref_axis',(0.70710678118653,0.,0.707106781186565));
#10082=DIRECTION('',(0.70710678118653,0.,0.707106781186565));
#10083=DIRECTION('',(-0.707106781186547,0.707106781186548,-2.51214793389404E-14));
#10084=DIRECTION('',(0.,-0.707106781186543,-0.707106781186552));
#10085=DIRECTION('center_axis',(-0.707106781186548,-0.707106781186547,0.));
#10086=DIRECTION('ref_axis',(0.,0.,1.));
#10087=DIRECTION('center_axis',(0.707106781186548,0.707106781186547,0.));
#10088=DIRECTION('ref_axis',(-0.707106781186547,0.707106781186548,0.));
#10089=DIRECTION('',(0.,0.,1.));
#10090=DIRECTION('',(0.,0.,-1.));
#10091=DIRECTION('center_axis',(0.,-0.707106781186552,0.707106781186543));
#10092=DIRECTION('ref_axis',(1.,0.,0.));
#10093=DIRECTION('',(-1.,0.,0.));
#10094=DIRECTION('',(1.,0.,0.));
#10095=DIRECTION('center_axis',(0.577350269189623,0.577350269189631,0.577350269189623));
#10096=DIRECTION('ref_axis',(0.707106781186548,0.,-0.707106781186548));
#10097=DIRECTION('',(0.707106781186552,-0.707106781186543,0.));
#10098=DIRECTION('',(0.,0.707106781186543,-0.707106781186552));
#10099=DIRECTION('',(-0.707106781186547,0.,0.707106781186547));
#10100=DIRECTION('center_axis',(-0.577350269189642,0.577350269189621,0.577350269189614));
#10101=DIRECTION('ref_axis',(0.70710678118653,0.,0.707106781186565));
#10102=DIRECTION('',(0.,-0.707106781186543,0.707106781186552));
#10103=DIRECTION('',(0.707106781186547,0.707106781186548,2.51214793389404E-14));
#10104=DIRECTION('',(-0.70710678118653,0.,-0.707106781186565));
#10105=DIRECTION('center_axis',(-0.707106781186548,0.707106781186547,0.));
#10106=DIRECTION('ref_axis',(0.,0.,1.));
#10107=DIRECTION('center_axis',(0.707106781186548,-0.707106781186547,0.));
#10108=DIRECTION('ref_axis',(0.707106781186547,0.707106781186548,0.));
#10109=DIRECTION('',(0.,0.,1.));
#10110=DIRECTION('',(0.,0.,-1.));
#10111=DIRECTION('center_axis',(-0.707106781186565,0.,0.70710678118653));
#10112=DIRECTION('ref_axis',(0.70710678118653,0.,0.707106781186565));
#10113=DIRECTION('',(0.,1.,0.));
#10114=DIRECTION('',(0.,-1.,0.));
#10115=DIRECTION('center_axis',(0.,0.707106781186552,0.707106781186543));
#10116=DIRECTION('ref_axis',(1.,0.,0.));
#10117=DIRECTION('',(-1.,0.,0.));
#10118=DIRECTION('',(1.,0.,0.));
#10119=DIRECTION('center_axis',(0.707106781186548,0.,0.707106781186548));
#10120=DIRECTION('ref_axis',(0.707106781186548,0.,-0.707106781186548));
#10121=DIRECTION('',(0.,1.,0.));
#10122=DIRECTION('',(0.,-1.,0.));
#10123=DIRECTION('center_axis',(0.707106781186543,0.707106781186552,0.));
#10124=DIRECTION('ref_axis',(0.,0.,-1.));
#10125=DIRECTION('center_axis',(-0.707106781186543,-0.707106781186552,0.));
#10126=DIRECTION('ref_axis',(-0.707106781186552,0.707106781186543,0.));
#10127=DIRECTION('',(0.,0.,1.));
#10128=DIRECTION('',(0.,0.,-1.));
#10129=DIRECTION('center_axis',(0.707106781186543,-0.707106781186552,0.));
#10130=DIRECTION('ref_axis',(0.,0.,-1.));
#10131=DIRECTION('center_axis',(-0.707106781186543,0.707106781186552,0.));
#10132=DIRECTION('ref_axis',(0.707106781186552,0.707106781186543,0.));
#10133=DIRECTION('',(0.,0.,1.));
#10134=DIRECTION('',(0.,0.,-1.));
#10135=DIRECTION('center_axis',(0.,1.,0.));
#10136=DIRECTION('ref_axis',(0.,0.,1.));
#10137=DIRECTION('',(-1.,0.,0.));
#10138=DIRECTION('center_axis',(1.,0.,0.));
#10139=DIRECTION('ref_axis',(0.,0.,-1.));
#10140=DIRECTION('center_axis',(-1.,0.,0.));
#10141=DIRECTION('ref_axis',(0.,0.,-1.));
#10142=DIRECTION('center_axis',(0.,0.,1.));
#10143=DIRECTION('ref_axis',(0.,-1.,0.));
#10144=DIRECTION('center_axis',(1.,0.,0.));
#10145=DIRECTION('ref_axis',(0.,1.22464679914735E-16,1.));
#10146=DIRECTION('',(1.,0.,0.));
#10147=DIRECTION('center_axis',(1.,0.,0.));
#10148=DIRECTION('ref_axis',(0.,0.,-1.));
#10149=DIRECTION('center_axis',(1.,0.,0.));
#10150=DIRECTION('ref_axis',(0.,0.,-1.));
#10151=DIRECTION('center_axis',(0.,-1.,0.));
#10152=DIRECTION('ref_axis',(0.,0.,-1.));
#10153=DIRECTION('axis',(0.,0.,1.));
#10154=DIRECTION('refdir',(1.,0.,0.));
#10155=DIRECTION('center_axis',(0.707106781186548,0.707106781186547,0.));
#10156=DIRECTION('ref_axis',(0.,0.,-1.));
#10157=DIRECTION('',(0.707106781186547,-0.707106781186548,0.));
#10158=DIRECTION('',(0.,0.,-1.));
#10159=DIRECTION('',(-0.707106781186547,0.707106781186548,0.));
#10160=DIRECTION('',(0.,0.,1.));
#10161=DIRECTION('center_axis',(-1.,0.,0.));
#10162=DIRECTION('ref_axis',(0.,0.707106781186548,0.707106781186548));
#10163=DIRECTION('center_axis',(1.,0.,0.));
#10164=DIRECTION('ref_axis',(0.,0.707106781186548,0.707106781186548));
#10165=DIRECTION('',(0.707106781186555,0.,-0.70710678118654));
#10166=DIRECTION('center_axis',(-1.,0.,0.));
#10167=DIRECTION('ref_axis',(0.,0.707106781186548,0.707106781186548));
#10168=DIRECTION('center_axis',(0.70710678118654,0.,0.707106781186555));
#10169=DIRECTION('ref_axis',(0.707106781186555,0.,-0.70710678118654));
#10170=DIRECTION('',(0.707106781186555,0.,-0.70710678118654));
#10171=DIRECTION('',(0.,1.,0.));
#10172=DIRECTION('',(0.,-1.,0.));
#10173=DIRECTION('center_axis',(-1.,0.,0.));
#10174=DIRECTION('ref_axis',(0.,-0.707106781186548,0.707106781186548));
#10175=DIRECTION('center_axis',(1.,0.,0.));
#10176=DIRECTION('ref_axis',(0.,-0.707106781186548,0.707106781186548));
#10177=DIRECTION('',(0.707106781186539,0.707106781186556,0.));
#10178=DIRECTION('center_axis',(-1.,0.,0.));
#10179=DIRECTION('ref_axis',(0.,-0.707106781186548,0.707106781186548));
#10180=DIRECTION('center_axis',(0.707106781186548,-0.707106781186547,0.));
#10181=DIRECTION('ref_axis',(0.,0.,-1.));
#10182=DIRECTION('',(0.707106781186547,0.707106781186548,0.));
#10183=DIRECTION('',(0.,0.,1.));
#10184=DIRECTION('',(0.,0.,-1.));
#10185=DIRECTION('center_axis',(-1.,0.,0.));
#10186=DIRECTION('ref_axis',(0.,-0.707106781186547,-0.707106781186547));
#10187=DIRECTION('center_axis',(1.,0.,0.));
#10188=DIRECTION('ref_axis',(0.,-0.707106781186548,-0.707106781186548));
#10189=DIRECTION('',(0.707106781186539,0.,0.707106781186556));
#10190=DIRECTION('center_axis',(-1.,0.,0.));
#10191=DIRECTION('ref_axis',(0.,-0.707106781186547,-0.707106781186547));
#10192=DIRECTION('center_axis',(0.707106781186548,0.,-0.707106781186547));
#10193=DIRECTION('ref_axis',(-0.707106781186547,0.,-0.707106781186548));
#10194=DIRECTION('',(0.707106781186547,0.,0.707106781186548));
#10195=DIRECTION('',(0.,-1.,0.));
#10196=DIRECTION('',(0.,1.,0.));
#10197=DIRECTION('center_axis',(-1.,0.,0.));
#10198=DIRECTION('ref_axis',(0.,0.707106781186548,-0.707106781186547));
#10199=DIRECTION('center_axis',(1.,0.,0.));
#10200=DIRECTION('ref_axis',(0.,0.707106781186548,-0.707106781186547));
#10201=DIRECTION('center_axis',(-1.,0.,0.));
#10202=DIRECTION('ref_axis',(0.,0.707106781186548,-0.707106781186547));
#10203=DIRECTION('center_axis',(-1.,0.,0.));
#10204=DIRECTION('ref_axis',(0.,-0.707106781186548,0.707106781186548));
#10205=DIRECTION('',(-1.,0.,0.));
#10206=DIRECTION('center_axis',(-1.,0.,0.));
#10207=DIRECTION('ref_axis',(0.,-0.707106781186548,0.707106781186548));
#10208=DIRECTION('',(1.,0.,0.));
#10209=DIRECTION('center_axis',(0.,0.,1.));
#10210=DIRECTION('ref_axis',(0.,1.,0.));
#10211=DIRECTION('',(1.,0.,0.));
#10212=DIRECTION('',(0.,1.,0.));
#10213=DIRECTION('center_axis',(-1.,0.,0.));
#10214=DIRECTION('ref_axis',(0.,0.707106781186548,0.707106781186548));
#10215=DIRECTION('',(-1.,0.,0.));
#10216=DIRECTION('center_axis',(-1.,0.,0.));
#10217=DIRECTION('ref_axis',(0.,0.707106781186548,0.707106781186548));
#10218=DIRECTION('center_axis',(0.,1.,0.));
#10219=DIRECTION('ref_axis',(0.,0.,-1.));
#10220=DIRECTION('',(1.,0.,0.));
#10221=DIRECTION('',(0.,0.,-1.));
#10222=DIRECTION('center_axis',(1.,0.,0.));
#10223=DIRECTION('ref_axis',(0.,0.,-1.));
#10224=DIRECTION('center_axis',(-1.,0.,0.));
#10225=DIRECTION('ref_axis',(0.,0.,-1.));
#10226=DIRECTION('center_axis',(-1.,0.,0.));
#10227=DIRECTION('ref_axis',(0.,0.,-1.));
#10228=DIRECTION('center_axis',(-1.,0.,0.));
#10229=DIRECTION('ref_axis',(0.,0.,-1.));
#10230=DIRECTION('center_axis',(-1.,0.,0.));
#10231=DIRECTION('ref_axis',(0.,0.,-1.));
#10232=DIRECTION('center_axis',(-1.,0.,0.));
#10233=DIRECTION('ref_axis',(0.,0.,-1.));
#10234=DIRECTION('center_axis',(-0.382683432365091,-0.923879532511286,0.));
#10235=DIRECTION('ref_axis',(0.,0.,-1.));
#10236=DIRECTION('',(-0.923879532511286,0.382683432365092,0.));
#10237=DIRECTION('',(0.,0.,-1.));
#10238=DIRECTION('',(0.923879532511286,-0.382683432365091,0.));
#10239=DIRECTION('',(0.,0.,1.));
#10240=DIRECTION('center_axis',(1.,0.,0.));
#10241=DIRECTION('ref_axis',(0.,-0.707106781186547,0.707106781186548));
#10242=DIRECTION('',(-0.923879532511289,0.,-0.382683432365085));
#10243=DIRECTION('center_axis',(1.,0.,0.));
#10244=DIRECTION('ref_axis',(0.,-0.707106781186547,0.707106781186548));
#10245=DIRECTION('center_axis',(-0.382683432365079,0.,0.923879532511291));
#10246=DIRECTION('ref_axis',(0.923879532511291,0.,0.382683432365079));
#10247=DIRECTION('',(-0.92387953251129,0.,-0.382683432365081));
#10248=DIRECTION('',(0.,-1.,0.));
#10249=DIRECTION('center_axis',(1.,0.,0.));
#10250=DIRECTION('ref_axis',(0.,0.707106781186547,0.707106781186548));
#10251=DIRECTION('',(-0.923879532511288,-0.382683432365088,0.));
#10252=DIRECTION('center_axis',(1.,0.,0.));
#10253=DIRECTION('ref_axis',(0.,0.707106781186547,0.707106781186548));
#10254=DIRECTION('center_axis',(-0.382683432365091,0.923879532511286,0.));
#10255=DIRECTION('ref_axis',(0.,0.,1.));
#10256=DIRECTION('',(-0.923879532511286,-0.382683432365091,0.));
#10257=DIRECTION('',(0.,0.,1.));
#10258=DIRECTION('center_axis',(1.,0.,0.));
#10259=DIRECTION('ref_axis',(0.,0.707106781186548,-0.707106781186547));
#10260=DIRECTION('',(-0.92387953251129,0.,0.382683432365082));
#10261=DIRECTION('center_axis',(1.,0.,0.));
#10262=DIRECTION('ref_axis',(0.,0.707106781186548,-0.707106781186547));
#10263=DIRECTION('center_axis',(-1.,0.,0.));
#10264=DIRECTION('ref_axis',(0.,0.707106781186548,-0.707106781186547));
#10265=DIRECTION('center_axis',(-0.382683432365091,0.,-0.923879532511286));
#10266=DIRECTION('ref_axis',(-0.923879532511286,0.,0.382683432365091));
#10267=DIRECTION('',(0.,1.,0.));
#10268=DIRECTION('',(0.,-1.,0.));
#10269=DIRECTION('',(-0.923879532511286,0.,0.382683432365092));
#10270=DIRECTION('',(0.,1.,0.));
#10271=DIRECTION('',(-6.49886142244849E-16,1.,2.69191654116148E-16));
#10272=DIRECTION('center_axis',(1.,0.,0.));
#10273=DIRECTION('ref_axis',(0.,-0.707106781186547,-0.707106781186547));
#10274=DIRECTION('center_axis',(1.,0.,0.));
#10275=DIRECTION('ref_axis',(0.,-0.707106781186548,-0.707106781186548));
#10276=DIRECTION('center_axis',(-1.,0.,0.));
#10277=DIRECTION('ref_axis',(0.,-0.707106781186548,-0.707106781186548));
#10278=DIRECTION('center_axis',(0.,-1.,0.));
#10279=DIRECTION('ref_axis',(0.,0.,1.));
#10280=DIRECTION('',(-1.,0.,0.));
#10281=DIRECTION('center_axis',(1.,0.,0.));
#10282=DIRECTION('ref_axis',(0.,0.707106781186547,0.707106781186547));
#10283=DIRECTION('',(0.707106781186549,0.707106781186546,0.));
#10284=DIRECTION('center_axis',(-1.,0.,0.));
#10285=DIRECTION('ref_axis',(0.,0.707106781186547,0.707106781186548));
#10286=DIRECTION('',(0.707106781186542,0.,0.707106781186553));
#10287=DIRECTION('center_axis',(-0.707106781186546,0.707106781186549,0.));
#10288=DIRECTION('ref_axis',(0.,0.,1.));
#10289=DIRECTION('',(0.707106781186549,0.707106781186546,6.28036983473511E-15));
#10290=DIRECTION('',(0.,0.,-1.));
#10291=DIRECTION('center_axis',(1.,0.,0.));
#10292=DIRECTION('ref_axis',(0.,0.707106781186548,-0.707106781186547));
#10293=DIRECTION('',(0.707106781186549,0.,-0.707106781186546));
#10294=DIRECTION('center_axis',(-1.,0.,0.));
#10295=DIRECTION('ref_axis',(0.,0.707106781186548,-0.707106781186547));
#10296=DIRECTION('center_axis',(-0.707106781186546,0.,-0.707106781186549));
#10297=DIRECTION('ref_axis',(-0.707106781186549,0.,0.707106781186546));
#10298=DIRECTION('',(0.707106781186542,0.,-0.707106781186553));
#10299=DIRECTION('',(0.,-1.,0.));
#10300=DIRECTION('',(0.707106781186549,0.,-0.707106781186546));
#10301=DIRECTION('',(0.,1.,0.));
#10302=DIRECTION('',(-0.707106781186549,0.,0.707106781186546));
#10303=DIRECTION('',(0.,-1.,0.));
#10304=DIRECTION('',(0.707106781186549,9.8130778667736E-17,-0.707106781186546));
#10305=DIRECTION('',(-1.38777878078144E-16,1.,1.38777878078144E-16));
#10306=DIRECTION('',(-0.707106781186549,-9.8130778667736E-17,0.707106781186546));
#10307=DIRECTION('',(0.,1.,0.));
#10308=DIRECTION('center_axis',(-0.707106781186546,0.,-0.707106781186549));
#10309=DIRECTION('ref_axis',(-0.707106781186549,0.,0.707106781186546));
#10310=DIRECTION('',(0.,-1.,0.));
#10311=DIRECTION('',(1.,0.,0.));
#10312=DIRECTION('center_axis',(-0.923879532511287,-4.97401319121531E-16,
-0.382683432365089));
#10313=DIRECTION('ref_axis',(-0.382683432365089,0.,0.923879532511287));
#10314=DIRECTION('',(-9.19077796360991E-16,1.,9.19077796360989E-16));
#10315=DIRECTION('center_axis',(-1.,0.,0.));
#10316=DIRECTION('ref_axis',(0.,0.,-1.));
#10317=DIRECTION('center_axis',(1.,-1.42859248789192E-15,0.));
#10318=DIRECTION('ref_axis',(0.,0.,-1.));
#10319=DIRECTION('',(-0.382683432365103,-1.13142611228769E-16,0.923879532511281));
#10320=DIRECTION('center_axis',(-1.,0.,0.));
#10321=DIRECTION('ref_axis',(0.,0.,-1.));
#10322=DIRECTION('center_axis',(-1.,0.,0.));
#10323=DIRECTION('ref_axis',(0.,0.,-1.));
#10324=DIRECTION('center_axis',(1.,0.,0.));
#10325=DIRECTION('ref_axis',(0.,-0.707106781186548,-0.707106781186548));
#10326=DIRECTION('',(0.38268343236509,0.,-0.923879532511287));
#10327=DIRECTION('center_axis',(-1.,0.,0.));
#10328=DIRECTION('ref_axis',(0.,-0.707106781186548,-0.707106781186548));
#10329=DIRECTION('',(0.382683432365099,-0.923879532511283,0.));
#10330=DIRECTION('center_axis',(-0.923879532511282,0.,-0.382683432365101));
#10331=DIRECTION('ref_axis',(-0.382683432365101,0.,0.923879532511282));
#10332=DIRECTION('',(0.,1.,0.));
#10333=DIRECTION('',(0.382683432365101,0.,-0.923879532511282));
#10334=DIRECTION('',(0.,1.,0.));
#10335=DIRECTION('',(0.382683432365101,0.,-0.923879532511282));
#10336=DIRECTION('center_axis',(-1.,0.,0.));
#10337=DIRECTION('ref_axis',(0.,0.,-1.));
#10338=DIRECTION('',(0.707106781186548,-8.65956056235493E-17,-0.707106781186547));
#10339=DIRECTION('center_axis',(1.,0.,0.));
#10340=DIRECTION('ref_axis',(0.,0.,-1.));
#10341=DIRECTION('center_axis',(-1.,0.,0.));
#10342=DIRECTION('ref_axis',(0.,0.,-1.));
#10343=DIRECTION('center_axis',(1.,-1.42859248789192E-15,0.));
#10344=DIRECTION('ref_axis',(0.,0.,-1.));
#10345=DIRECTION('',(-0.382683432365103,-1.13142611228769E-16,0.923879532511281));
#10346=DIRECTION('center_axis',(-1.,0.,0.));
#10347=DIRECTION('ref_axis',(0.,0.,-1.));
#10348=DIRECTION('center_axis',(-1.,0.,0.));
#10349=DIRECTION('ref_axis',(0.,0.,-1.));
#10350=DIRECTION('center_axis',(1.,0.,0.));
#10351=DIRECTION('ref_axis',(0.,0.707106781186548,-0.707106781186547));
#10352=DIRECTION('',(0.382683432365085,0.923879532511289,-1.2016967424393E-14));
#10353=DIRECTION('',(0.382683432365099,0.,-0.923879532511283));
#10354=DIRECTION('center_axis',(-0.923879532511282,0.382683432365101,0.));
#10355=DIRECTION('ref_axis',(0.,0.,1.));
#10356=DIRECTION('',(0.,0.,1.));
#10357=DIRECTION('',(0.382683432365099,0.923879532511283,0.));
#10358=DIRECTION('center_axis',(-1.,0.,0.));
#10359=DIRECTION('ref_axis',(0.,0.,-1.));
#10360=DIRECTION('',(0.707106781186548,-8.65956056235493E-17,-0.707106781186547));
#10361=DIRECTION('center_axis',(1.,0.,0.));
#10362=DIRECTION('ref_axis',(0.,0.,-1.));
#10363=DIRECTION('center_axis',(-1.,0.,0.));
#10364=DIRECTION('ref_axis',(0.,0.,-1.));
#10365=DIRECTION('center_axis',(1.,-1.60716654887841E-15,0.));
#10366=DIRECTION('ref_axis',(0.,0.,-1.));
#10367=DIRECTION('',(-0.382683432365116,-1.13142611228769E-16,0.923879532511276));
#10368=DIRECTION('center_axis',(-1.,0.,0.));
#10369=DIRECTION('ref_axis',(0.,0.,-1.));
#10370=DIRECTION('center_axis',(-0.923879532511282,-0.382683432365101,0.));
#10371=DIRECTION('ref_axis',(0.,0.,1.));
#10372=DIRECTION('',(0.,0.,1.));
#10373=DIRECTION('',(0.3826834323651,-0.923879532511283,0.));
#10374=DIRECTION('',(0.,0.,-1.));
#10375=DIRECTION('center_axis',(-1.,0.,0.));
#10376=DIRECTION('ref_axis',(0.,0.,1.));
#10377=DIRECTION('',(0.,-1.,0.));
#10378=DIRECTION('center_axis',(-1.,0.,0.));
#10379=DIRECTION('ref_axis',(0.,0.,-1.));
#10380=DIRECTION('',(0.,1.,0.));
#10381=DIRECTION('',(0.,-1.69953884180861E-32,1.));
#10382=DIRECTION('',(0.,-1.,0.));
#10383=DIRECTION('',(0.,1.69953884180861E-32,-1.));
#10384=DIRECTION('',(0.,1.,0.));
#10385=DIRECTION('',(0.,1.69953884180861E-32,-1.));
#10386=DIRECTION('',(0.,-1.,0.));
#10387=DIRECTION('',(0.,1.69953884180861E-32,-1.));
#10388=DIRECTION('',(0.,1.,0.));
#10389=DIRECTION('',(0.,0.,1.));
#10390=DIRECTION('',(0.,-1.,0.));
#10391=DIRECTION('',(0.,0.,-1.));
#10392=DIRECTION('',(0.,1.,0.));
#10393=DIRECTION('',(0.,0.,-1.));
#10394=DIRECTION('',(0.,-1.,0.));
#10395=DIRECTION('',(0.,0.,-1.));
#10396=DIRECTION('',(0.,1.,0.));
#10397=DIRECTION('',(0.,0.,-1.));
#10398=DIRECTION('',(0.,1.,0.));
#10399=DIRECTION('',(0.,0.,1.));
#10400=DIRECTION('',(0.,-1.,0.));
#10401=DIRECTION('',(0.,0.,-1.));
#10402=DIRECTION('',(0.,1.,0.));
#10403=DIRECTION('',(0.,0.,-1.));
#10404=DIRECTION('',(0.,-1.,0.));
#10405=DIRECTION('',(0.,0.,-1.));
#10406=DIRECTION('',(0.,1.,0.));
#10407=DIRECTION('',(0.,1.69953884180861E-32,-1.));
#10408=DIRECTION('',(0.,1.,0.));
#10409=DIRECTION('',(0.,-1.69953884180861E-32,1.));
#10410=DIRECTION('',(0.,-1.,0.));
#10411=DIRECTION('',(0.,1.69953884180861E-32,-1.));
#10412=DIRECTION('',(0.,1.,0.));
#10413=DIRECTION('',(0.,1.69953884180861E-32,-1.));
#10414=DIRECTION('',(0.,-1.,0.));
#10415=DIRECTION('',(0.,1.69953884180861E-32,-1.));
#10416=DIRECTION('',(0.,0.55569909667333,0.831383493916282));
#10417=DIRECTION('',(0.,0.,-1.));
#10418=DIRECTION('',(0.,1.,0.));
#10419=DIRECTION('',(0.,0.,1.));
#10420=DIRECTION('',(0.,-1.,0.));
#10421=DIRECTION('',(0.,-0.556032657337733,-0.831160444182673));
#10422=DIRECTION('',(0.,0.,1.));
#10423=DIRECTION('',(0.,-1.,0.));
#10424=DIRECTION('',(0.,0.,-1.));
#10425=DIRECTION('',(0.,1.,0.));
#10426=DIRECTION('center_axis',(1.,0.,0.));
#10427=DIRECTION('ref_axis',(0.,0.,-1.));
#10428=DIRECTION('',(0.,0.55569909667333,0.831383493916282));
#10429=DIRECTION('',(0.,0.,-1.));
#10430=DIRECTION('',(0.,1.,0.));
#10431=DIRECTION('',(0.,0.,1.));
#10432=DIRECTION('',(0.,-1.,0.));
#10433=DIRECTION('',(0.,-0.556032657337733,-0.831160444182673));
#10434=DIRECTION('',(0.,0.,1.));
#10435=DIRECTION('',(0.,-1.,0.));
#10436=DIRECTION('',(0.,0.,-1.));
#10437=DIRECTION('',(0.,1.,0.));
#10438=DIRECTION('center_axis',(-1.,0.,0.));
#10439=DIRECTION('ref_axis',(0.,0.,-1.));
#10440=DIRECTION('',(0.707106781186547,-8.65956056235494E-17,-0.707106781186548));
#10441=DIRECTION('center_axis',(1.,0.,0.));
#10442=DIRECTION('ref_axis',(0.,0.,-1.));
#10443=DIRECTION('center_axis',(-1.,0.,0.));
#10444=DIRECTION('ref_axis',(0.,0.,-1.));
#10445=DIRECTION('center_axis',(1.,-1.60716654887841E-15,0.));
#10446=DIRECTION('ref_axis',(0.,0.,-1.));
#10447=DIRECTION('',(-0.382683432365116,-1.13142611228769E-16,0.923879532511276));
#10448=DIRECTION('center_axis',(-1.,0.,0.));
#10449=DIRECTION('ref_axis',(0.,0.,-1.));
#10450=DIRECTION('',(0.707106781186547,-8.65956056235494E-17,-0.707106781186548));
#10451=DIRECTION('center_axis',(1.,0.,0.));
#10452=DIRECTION('ref_axis',(0.,0.,-1.));
#10453=DIRECTION('center_axis',(-0.923879532511282,0.,-0.382683432365101));
#10454=DIRECTION('ref_axis',(-0.382683432365101,0.,0.923879532511282));
#10455=DIRECTION('',(-0.382683432365101,0.,0.923879532511282));
#10456=DIRECTION('',(0.382683432365101,5.31079947192899E-17,-0.923879532511282));
#10457=DIRECTION('',(0.,1.,0.));
#10458=DIRECTION('',(0.382683432365101,5.31079947192899E-17,-0.923879532511282));
#10459=DIRECTION('center_axis',(1.38777878078144E-16,-1.,-1.69953884180861E-32));
#10460=DIRECTION('ref_axis',(-1.22464679914735E-16,0.,-1.));
#10461=DIRECTION('',(1.,1.38777878078144E-16,0.));
#10462=DIRECTION('',(-1.22464679914735E-16,0.,-1.));
#10463=DIRECTION('center_axis',(0.,0.,-1.));
#10464=DIRECTION('ref_axis',(-1.22464679914735E-16,1.,0.));
#10465=DIRECTION('',(1.,1.38777878078144E-16,0.));
#10466=DIRECTION('',(-1.22464679914735E-16,1.,0.));
#10467=DIRECTION('center_axis',(-0.923879532511282,0.,-0.382683432365101));
#10468=DIRECTION('ref_axis',(-0.382683432365101,0.,0.923879532511282));
#10469=DIRECTION('center_axis',(1.,0.,0.));
#10470=DIRECTION('ref_axis',(0.,0.707106781186547,0.707106781186548));
#10471=DIRECTION('',(0.382683432365096,-1.20169674243929E-14,0.923879532511284));
#10472=DIRECTION('center_axis',(-0.923879532511287,0.,0.38268343236509));
#10473=DIRECTION('ref_axis',(0.38268343236509,0.,0.923879532511286));
#10474=DIRECTION('',(0.382683432365112,0.,0.923879532511278));
#10475=DIRECTION('',(0.,1.,0.));
#10476=DIRECTION('center_axis',(1.,0.,0.));
#10477=DIRECTION('ref_axis',(7.9970871068614E-17,-0.707106781186547,0.707106781186548));
#10478=DIRECTION('center_axis',(-1.,-2.15587857746042E-16,0.));
#10479=DIRECTION('ref_axis',(1.52443636153707E-16,-0.707106781186547,0.707106781186548));
#10480=DIRECTION('center_axis',(-0.707106781186546,0.,0.707106781186549));
#10481=DIRECTION('ref_axis',(0.707106781186549,0.,0.707106781186546));
#10482=DIRECTION('',(-0.707106781186542,0.,-0.707106781186553));
#10483=DIRECTION('center_axis',(1.,0.,0.));
#10484=DIRECTION('ref_axis',(0.,-0.707106781186547,0.707106781186547));
#10485=DIRECTION('',(0.707106781186542,-0.707106781186553,0.));
#10486=DIRECTION('center_axis',(-0.707106781186546,-0.707106781186549,0.));
#10487=DIRECTION('ref_axis',(0.,0.,1.));
#10488=DIRECTION('',(0.707106781186549,-0.707106781186546,0.));
#10489=DIRECTION('center_axis',(1.,0.,0.));
#10490=DIRECTION('ref_axis',(0.,-0.707106781186547,-0.707106781186547));
#10491=DIRECTION('center_axis',(0.,-1.,0.));
#10492=DIRECTION('ref_axis',(-1.22464679914735E-16,0.,-1.));
#10493=DIRECTION('',(1.,0.,0.));
#10494=DIRECTION('',(-1.22464679914735E-16,0.,-1.));
#10495=DIRECTION('center_axis',(0.,0.,-1.));
#10496=DIRECTION('ref_axis',(-1.22464679914735E-16,1.,0.));
#10497=DIRECTION('',(1.,0.,0.));
#10498=DIRECTION('',(-1.22464679914735E-16,1.,0.));
#10499=DIRECTION('center_axis',(-1.,-9.19077796360991E-16,-2.78913508712442E-16));
#10500=DIRECTION('ref_axis',(-2.78913508712442E-16,0.,1.));
#10501=DIRECTION('center_axis',(0.,-1.,0.));
#10502=DIRECTION('ref_axis',(-1.22464679914735E-16,0.,-1.));
#10503=DIRECTION('',(1.,0.,0.));
#10504=DIRECTION('',(-1.22464679914735E-16,0.,-1.));
#10505=DIRECTION('center_axis',(0.,0.,1.));
#10506=DIRECTION('ref_axis',(1.22464679914735E-16,-1.,0.));
#10507=DIRECTION('',(1.,0.,0.));
#10508=DIRECTION('',(1.22464679914735E-16,-1.,0.));
#10509=DIRECTION('center_axis',(0.,-1.,0.));
#10510=DIRECTION('ref_axis',(-1.22464679914735E-16,0.,-1.));
#10511=DIRECTION('',(1.,0.,0.));
#10512=DIRECTION('',(-1.22464679914735E-16,0.,-1.));
#10513=DIRECTION('center_axis',(0.,0.,-1.));
#10514=DIRECTION('ref_axis',(-1.22464679914735E-16,1.,0.));
#10515=DIRECTION('',(1.,0.,0.));
#10516=DIRECTION('',(-1.22464679914735E-16,1.,0.));
#10517=DIRECTION('center_axis',(0.,-1.,0.));
#10518=DIRECTION('ref_axis',(-1.22464679914735E-16,0.,-1.));
#10519=DIRECTION('',(1.,0.,0.));
#10520=DIRECTION('',(-1.22464679914735E-16,0.,-1.));
#10521=DIRECTION('center_axis',(0.,0.,1.));
#10522=DIRECTION('ref_axis',(1.22464679914735E-16,-1.,0.));
#10523=DIRECTION('',(1.,0.,0.));
#10524=DIRECTION('',(1.22464679914735E-16,-1.,0.));
#10525=DIRECTION('center_axis',(0.,1.,0.));
#10526=DIRECTION('ref_axis',(1.22464679914735E-16,0.,1.));
#10527=DIRECTION('',(1.22464679914735E-16,0.,1.));
#10528=DIRECTION('center_axis',(1.,0.,0.));
#10529=DIRECTION('ref_axis',(0.,0.,-1.));
#10530=DIRECTION('center_axis',(1.38777878078144E-16,-1.,-1.69953884180861E-32));
#10531=DIRECTION('ref_axis',(-1.22464679914735E-16,0.,-1.));
#10532=DIRECTION('',(1.,1.38777878078144E-16,0.));
#10533=DIRECTION('',(-1.22464679914735E-16,0.,-1.));
#10534=DIRECTION('center_axis',(0.,0.,1.));
#10535=DIRECTION('ref_axis',(1.22464679914735E-16,-1.,0.));
#10536=DIRECTION('',(1.,1.38777878078144E-16,0.));
#10537=DIRECTION('',(1.22464679914735E-16,-1.,0.));
#10538=DIRECTION('center_axis',(1.38777878078144E-16,-1.,-1.69953884180861E-32));
#10539=DIRECTION('ref_axis',(-1.22464679914735E-16,0.,-1.));
#10540=DIRECTION('',(1.,1.38777878078144E-16,0.));
#10541=DIRECTION('',(-1.22464679914735E-16,0.,-1.));
#10542=DIRECTION('center_axis',(0.,0.,-1.));
#10543=DIRECTION('ref_axis',(-1.22464679914735E-16,1.,0.));
#10544=DIRECTION('',(1.,1.38777878078144E-16,0.));
#10545=DIRECTION('',(-1.22464679914735E-16,1.,0.));
#10546=DIRECTION('center_axis',(1.38777878078144E-16,-1.,-1.69953884180861E-32));
#10547=DIRECTION('ref_axis',(-1.22464679914735E-16,0.,-1.));
#10548=DIRECTION('',(1.,1.38777878078144E-16,0.));
#10549=DIRECTION('',(-1.22464679914735E-16,0.,-1.));
#10550=DIRECTION('center_axis',(0.,0.,1.));
#10551=DIRECTION('ref_axis',(1.22464679914735E-16,-1.,0.));
#10552=DIRECTION('',(1.,1.38777878078144E-16,0.));
#10553=DIRECTION('',(1.22464679914735E-16,-1.,0.));
#10554=DIRECTION('center_axis',(-1.38777878078144E-16,1.,1.69953884180861E-32));
#10555=DIRECTION('ref_axis',(1.22464679914735E-16,0.,1.));
#10556=DIRECTION('',(1.22464679914735E-16,0.,1.));
#10557=DIRECTION('center_axis',(1.,1.38777878078144E-16,0.));
#10558=DIRECTION('ref_axis',(0.,0.,-1.));
#10559=DIRECTION('',(1.,0.,0.));
#10560=DIRECTION('',(1.,0.,0.));
#10561=DIRECTION('',(1.,0.,0.));
#10562=DIRECTION('',(1.,0.,0.));
#10563=DIRECTION('',(1.,0.,0.));
#10564=DIRECTION('center_axis',(0.,0.,-1.));
#10565=DIRECTION('ref_axis',(-1.22464679914735E-16,1.,0.));
#10566=DIRECTION('',(1.,0.,0.));
#10567=DIRECTION('',(-1.22464679914735E-16,1.,0.));
#10568=DIRECTION('',(1.,0.,0.));
#10569=DIRECTION('center_axis',(0.,-1.,0.));
#10570=DIRECTION('ref_axis',(-1.22464679914735E-16,0.,-1.));
#10571=DIRECTION('',(1.,0.,0.));
#10572=DIRECTION('',(-1.22464679914735E-16,0.,-1.));
#10573=DIRECTION('center_axis',(0.,0.,1.));
#10574=DIRECTION('ref_axis',(1.22464679914735E-16,-1.,0.));
#10575=DIRECTION('',(1.,0.,0.));
#10576=DIRECTION('',(1.22464679914735E-16,-1.,0.));
#10577=DIRECTION('center_axis',(0.,-1.,0.));
#10578=DIRECTION('ref_axis',(-1.22464679914735E-16,0.,-1.));
#10579=DIRECTION('',(1.,0.,0.));
#10580=DIRECTION('',(-1.22464679914735E-16,0.,-1.));
#10581=DIRECTION('center_axis',(0.,0.,-1.));
#10582=DIRECTION('ref_axis',(-1.22464679914735E-16,1.,0.));
#10583=DIRECTION('',(1.,0.,0.));
#10584=DIRECTION('',(-1.22464679914735E-16,1.,0.));
#10585=DIRECTION('center_axis',(0.,-1.,0.));
#10586=DIRECTION('ref_axis',(-1.22464679914735E-16,0.,-1.));
#10587=DIRECTION('',(1.,0.,0.));
#10588=DIRECTION('',(-1.22464679914735E-16,0.,-1.));
#10589=DIRECTION('center_axis',(0.,0.,1.));
#10590=DIRECTION('ref_axis',(1.22464679914735E-16,-1.,0.));
#10591=DIRECTION('',(1.,0.,0.));
#10592=DIRECTION('',(1.22464679914735E-16,-1.,0.));
#10593=DIRECTION('center_axis',(0.,1.,0.));
#10594=DIRECTION('ref_axis',(1.22464679914735E-16,0.,1.));
#10595=DIRECTION('',(1.,0.,0.));
#10596=DIRECTION('',(1.22464679914735E-16,0.,1.));
#10597=DIRECTION('center_axis',(0.,0.,-1.));
#10598=DIRECTION('ref_axis',(-1.22464679914735E-16,1.,0.));
#10599=DIRECTION('',(1.,0.,0.));
#10600=DIRECTION('',(-1.22464679914735E-16,1.,0.));
#10601=DIRECTION('center_axis',(0.,-1.,0.));
#10602=DIRECTION('ref_axis',(-1.22464679914735E-16,0.,-1.));
#10603=DIRECTION('',(-1.22464679914735E-16,0.,-1.));
#10604=DIRECTION('center_axis',(1.,0.,0.));
#10605=DIRECTION('ref_axis',(0.,0.,-1.));
#10606=DIRECTION('center_axis',(0.,0.,-1.));
#10607=DIRECTION('ref_axis',(-1.22464679914735E-16,1.,0.));
#10608=DIRECTION('',(1.,1.38777878078144E-16,0.));
#10609=DIRECTION('',(-1.22464679914735E-16,1.,0.));
#10610=DIRECTION('',(1.,1.38777878078144E-16,0.));
#10611=DIRECTION('center_axis',(1.38777878078144E-16,-1.,-1.69953884180861E-32));
#10612=DIRECTION('ref_axis',(-1.22464679914735E-16,0.,-1.));
#10613=DIRECTION('',(1.,1.38777878078144E-16,0.));
#10614=DIRECTION('',(-1.22464679914735E-16,0.,-1.));
#10615=DIRECTION('center_axis',(0.,0.,1.));
#10616=DIRECTION('ref_axis',(1.22464679914735E-16,-1.,0.));
#10617=DIRECTION('',(1.,1.38777878078144E-16,0.));
#10618=DIRECTION('',(1.22464679914735E-16,-1.,0.));
#10619=DIRECTION('center_axis',(1.38777878078144E-16,-1.,-1.69953884180861E-32));
#10620=DIRECTION('ref_axis',(-1.22464679914735E-16,0.,-1.));
#10621=DIRECTION('',(1.,1.38777878078144E-16,0.));
#10622=DIRECTION('',(-1.22464679914735E-16,0.,-1.));
#10623=DIRECTION('center_axis',(0.,0.,-1.));
#10624=DIRECTION('ref_axis',(-1.22464679914735E-16,1.,0.));
#10625=DIRECTION('',(1.,1.38777878078144E-16,0.));
#10626=DIRECTION('',(-1.22464679914735E-16,1.,0.));
#10627=DIRECTION('center_axis',(1.38777878078144E-16,-1.,-1.69953884180861E-32));
#10628=DIRECTION('ref_axis',(-1.22464679914735E-16,0.,-1.));
#10629=DIRECTION('',(1.,1.38777878078144E-16,0.));
#10630=DIRECTION('',(-1.22464679914735E-16,0.,-1.));
#10631=DIRECTION('center_axis',(0.,0.,1.));
#10632=DIRECTION('ref_axis',(1.22464679914735E-16,-1.,0.));
#10633=DIRECTION('',(1.,1.38777878078144E-16,0.));
#10634=DIRECTION('',(1.22464679914735E-16,-1.,0.));
#10635=DIRECTION('center_axis',(-1.38777878078144E-16,1.,1.69953884180861E-32));
#10636=DIRECTION('ref_axis',(1.22464679914735E-16,0.,1.));
#10637=DIRECTION('',(1.,1.38777878078144E-16,0.));
#10638=DIRECTION('',(1.22464679914735E-16,0.,1.));
#10639=DIRECTION('center_axis',(0.,0.,-1.));
#10640=DIRECTION('ref_axis',(-1.22464679914735E-16,1.,0.));
#10641=DIRECTION('',(1.,1.38777878078144E-16,0.));
#10642=DIRECTION('',(-1.22464679914735E-16,1.,0.));
#10643=DIRECTION('center_axis',(1.38777878078144E-16,-1.,-1.69953884180861E-32));
#10644=DIRECTION('ref_axis',(-1.22464679914735E-16,0.,-1.));
#10645=DIRECTION('',(-1.22464679914735E-16,0.,-1.));
#10646=DIRECTION('center_axis',(1.,1.38777878078144E-16,0.));
#10647=DIRECTION('ref_axis',(0.,0.,-1.));
#10648=DIRECTION('',(1.,0.,0.));
#10649=DIRECTION('',(1.,0.,0.));
#10650=DIRECTION('',(1.,0.,0.));
#10651=DIRECTION('',(1.,0.,0.));
#10652=DIRECTION('',(1.,0.,0.));
#10653=DIRECTION('',(1.,0.,0.));
#10654=DIRECTION('',(1.,0.,0.));
#10655=DIRECTION('',(1.,0.,0.));
#10656=DIRECTION('',(1.,0.,0.));
#10657=DIRECTION('',(1.,0.,0.));
#10658=DIRECTION('',(1.,0.,0.));
#10659=DIRECTION('center_axis',(-1.,-9.19077796360991E-16,-2.78913508712442E-16));
#10660=DIRECTION('ref_axis',(-2.78913508712442E-16,0.,1.));
#10661=DIRECTION('center_axis',(0.,0.831383493916282,-0.55569909667333));
#10662=DIRECTION('ref_axis',(3.37616014658449E-17,0.55569909667333,0.831383493916282));
#10663=DIRECTION('',(1.,0.,0.));
#10664=DIRECTION('',(3.37616014658449E-17,0.55569909667333,0.831383493916282));
#10665=DIRECTION('',(1.,0.,0.));
#10666=DIRECTION('center_axis',(0.,0.,-1.));
#10667=DIRECTION('ref_axis',(-1.22464679914735E-16,1.,0.));
#10668=DIRECTION('',(1.,0.,0.));
#10669=DIRECTION('',(-1.22464679914735E-16,1.,0.));
#10670=DIRECTION('center_axis',(0.,-1.,0.));
#10671=DIRECTION('ref_axis',(-1.22464679914735E-16,0.,-1.));
#10672=DIRECTION('',(1.,0.,0.));
#10673=DIRECTION('',(-1.22464679914735E-16,0.,-1.));
#10674=DIRECTION('center_axis',(0.,0.,1.));
#10675=DIRECTION('ref_axis',(1.22464679914735E-16,-1.,0.));
#10676=DIRECTION('',(1.,0.,0.));
#10677=DIRECTION('',(1.22464679914735E-16,-1.,0.));
#10678=DIRECTION('center_axis',(0.,1.,0.));
#10679=DIRECTION('ref_axis',(1.22464679914735E-16,0.,1.));
#10680=DIRECTION('',(1.,0.,0.));
#10681=DIRECTION('',(1.22464679914735E-16,0.,1.));
#10682=DIRECTION('center_axis',(0.,-0.831160444182673,0.556032657337733));
#10683=DIRECTION('ref_axis',(-3.36934363516151E-17,-0.556032657337733,-0.831160444182673));
#10684=DIRECTION('',(1.,0.,0.));
#10685=DIRECTION('',(-3.36934363516151E-17,-0.556032657337733,-0.831160444182673));
#10686=DIRECTION('center_axis',(0.,0.,1.));
#10687=DIRECTION('ref_axis',(1.22464679914735E-16,-1.,0.));
#10688=DIRECTION('',(1.,0.,0.));
#10689=DIRECTION('',(1.22464679914735E-16,-1.,0.));
#10690=DIRECTION('center_axis',(0.,1.,0.));
#10691=DIRECTION('ref_axis',(1.22464679914735E-16,0.,1.));
#10692=DIRECTION('',(1.,0.,0.));
#10693=DIRECTION('',(1.22464679914735E-16,0.,1.));
#10694=DIRECTION('center_axis',(0.,0.,-1.));
#10695=DIRECTION('ref_axis',(-1.22464679914735E-16,1.,0.));
#10696=DIRECTION('',(1.,0.,0.));
#10697=DIRECTION('',(-1.22464679914735E-16,1.,0.));
#10698=DIRECTION('center_axis',(0.,-1.,0.));
#10699=DIRECTION('ref_axis',(-1.22464679914735E-16,0.,-1.));
#10700=DIRECTION('',(-1.22464679914735E-16,0.,-1.));
#10701=DIRECTION('center_axis',(1.,0.,0.));
#10702=DIRECTION('ref_axis',(0.,0.,-1.));
#10703=DIRECTION('',(1.,0.,0.));
#10704=DIRECTION('',(1.,0.,0.));
#10705=DIRECTION('',(1.,0.,0.));
#10706=DIRECTION('',(1.,0.,0.));
#10707=DIRECTION('',(1.,0.,0.));
#10708=DIRECTION('',(1.,0.,0.));
#10709=DIRECTION('',(1.,0.,0.));
#10710=DIRECTION('',(1.,0.,0.));
#10711=DIRECTION('',(1.,0.,0.));
#10712=DIRECTION('',(1.,0.,0.));
#10713=DIRECTION('',(1.,0.,0.));
#10714=DIRECTION('center_axis',(-1.,-9.1907723979186E-16,-2.78913274147473E-16));
#10715=DIRECTION('ref_axis',(-2.78913274147473E-16,0.,1.));
#10716=DIRECTION('center_axis',(0.,0.831383493916282,-0.55569909667333));
#10717=DIRECTION('ref_axis',(3.37616014658449E-17,0.55569909667333,0.831383493916282));
#10718=DIRECTION('',(1.,0.,0.));
#10719=DIRECTION('',(3.37616014658449E-17,0.55569909667333,0.831383493916282));
#10720=DIRECTION('',(1.,0.,0.));
#10721=DIRECTION('center_axis',(0.,0.,-1.));
#10722=DIRECTION('ref_axis',(-1.22464679914735E-16,1.,0.));
#10723=DIRECTION('',(1.,0.,0.));
#10724=DIRECTION('',(-1.22464679914735E-16,1.,0.));
#10725=DIRECTION('center_axis',(0.,-1.,0.));
#10726=DIRECTION('ref_axis',(-1.22464679914735E-16,0.,-1.));
#10727=DIRECTION('',(1.,0.,0.));
#10728=DIRECTION('',(-1.22464679914735E-16,0.,-1.));
#10729=DIRECTION('center_axis',(0.,0.,1.));
#10730=DIRECTION('ref_axis',(1.22464679914735E-16,-1.,0.));
#10731=DIRECTION('',(1.,0.,0.));
#10732=DIRECTION('',(1.22464679914735E-16,-1.,0.));
#10733=DIRECTION('center_axis',(0.,1.,0.));
#10734=DIRECTION('ref_axis',(1.22464679914735E-16,0.,1.));
#10735=DIRECTION('',(1.,0.,0.));
#10736=DIRECTION('',(1.22464679914735E-16,0.,1.));
#10737=DIRECTION('center_axis',(0.,-0.831160444182673,0.556032657337733));
#10738=DIRECTION('ref_axis',(-3.36934363516151E-17,-0.556032657337733,-0.831160444182673));
#10739=DIRECTION('',(1.,0.,0.));
#10740=DIRECTION('',(-3.36934363516151E-17,-0.556032657337733,-0.831160444182673));
#10741=DIRECTION('center_axis',(0.,0.,1.));
#10742=DIRECTION('ref_axis',(1.22464679914735E-16,-1.,0.));
#10743=DIRECTION('',(1.,0.,0.));
#10744=DIRECTION('',(1.22464679914735E-16,-1.,0.));
#10745=DIRECTION('center_axis',(0.,1.,0.));
#10746=DIRECTION('ref_axis',(1.22464679914735E-16,0.,1.));
#10747=DIRECTION('',(1.,0.,0.));
#10748=DIRECTION('',(1.22464679914735E-16,0.,1.));
#10749=DIRECTION('center_axis',(0.,0.,-1.));
#10750=DIRECTION('ref_axis',(-1.22464679914735E-16,1.,0.));
#10751=DIRECTION('',(1.,0.,0.));
#10752=DIRECTION('',(-1.22464679914735E-16,1.,0.));
#10753=DIRECTION('center_axis',(0.,-1.,0.));
#10754=DIRECTION('ref_axis',(-1.22464679914735E-16,0.,-1.));
#10755=DIRECTION('',(-1.22464679914735E-16,0.,-1.));
#10756=DIRECTION('center_axis',(1.,0.,0.));
#10757=DIRECTION('ref_axis',(0.,0.,-1.));
#10758=DIRECTION('',(1.,0.,0.));
#10759=DIRECTION('',(1.,0.,0.));
#10760=DIRECTION('',(1.,0.,0.));
#10761=DIRECTION('',(1.,0.,0.));
#10762=DIRECTION('',(1.,0.,0.));
#10763=DIRECTION('',(1.,0.,0.));
#10764=DIRECTION('',(1.,0.,0.));
#10765=DIRECTION('',(1.,0.,0.));
#10766=DIRECTION('',(1.,0.,0.));
#10767=DIRECTION('',(1.,0.,0.));
#10768=DIRECTION('',(1.,0.,0.));
#10769=DIRECTION('center_axis',(-1.,-9.19077239791859E-16,-2.78913274147473E-16));
#10770=DIRECTION('ref_axis',(-2.78913274147473E-16,0.,1.));
#10771=DIRECTION('center_axis',(1.,0.,0.));
#10772=DIRECTION('ref_axis',(0.,0.,-1.));
#10773=DIRECTION('',(1.,0.,0.));
#10774=DIRECTION('center_axis',(1.,0.,0.));
#10775=DIRECTION('ref_axis',(0.,0.,-1.));
#10776=DIRECTION('',(1.,0.,0.));
#10777=DIRECTION('center_axis',(1.,0.,0.));
#10778=DIRECTION('ref_axis',(0.,0.,-1.));
#10779=DIRECTION('',(1.,0.,0.));
#10780=DIRECTION('center_axis',(1.,0.,0.));
#10781=DIRECTION('ref_axis',(0.,0.,-1.));
#10782=DIRECTION('',(1.,0.,0.));
#10783=DIRECTION('center_axis',(1.,0.,0.));
#10784=DIRECTION('ref_axis',(0.,0.,-1.));
#10785=DIRECTION('',(1.,0.,0.));
#10786=DIRECTION('center_axis',(-1.,0.,0.));
#10787=DIRECTION('ref_axis',(0.,0.707106781186548,-0.707106781186547));
#10788=DIRECTION('',(-1.,0.,0.));
#10789=DIRECTION('center_axis',(-1.,0.,0.));
#10790=DIRECTION('ref_axis',(0.,-0.707106781186548,-0.707106781186548));
#10791=DIRECTION('',(1.,0.,0.));
#10792=DIRECTION('center_axis',(0.,0.,-1.));
#10793=DIRECTION('ref_axis',(0.,-1.,0.));
#10794=DIRECTION('axis',(0.,0.,1.));
#10795=DIRECTION('refdir',(1.,0.,0.));
#10796=DIRECTION('center_axis',(-0.707106781186555,-0.70710678118654,0.));
#10797=DIRECTION('ref_axis',(0.,0.,1.));
#10798=DIRECTION('',(0.70710678118654,-0.707106781186555,0.));
#10799=DIRECTION('',(0.,0.,1.));
#10800=DIRECTION('',(-0.70710678118654,0.707106781186555,0.));
#10801=DIRECTION('',(0.,0.,-1.));
#10802=DIRECTION('center_axis',(1.,0.,0.));
#10803=DIRECTION('ref_axis',(0.,-0.707106781186548,-0.707106781186547));
#10804=DIRECTION('',(0.70710678118654,0.,-0.707106781186555));
#10805=DIRECTION('center_axis',(-1.,0.,0.));
#10806=DIRECTION('ref_axis',(0.,-0.707106781186548,-0.707106781186547));
#10807=DIRECTION('center_axis',(1.,0.,0.));
#10808=DIRECTION('ref_axis',(0.,-0.707106781186548,-0.707106781186547));
#10809=DIRECTION('center_axis',(-0.707106781186548,0.,-0.707106781186548));
#10810=DIRECTION('ref_axis',(-0.707106781186548,0.,0.707106781186548));
#10811=DIRECTION('',(0.707106781186548,0.,-0.707106781186548));
#10812=DIRECTION('',(0.,-1.,0.));
#10813=DIRECTION('',(0.,1.,0.));
#10814=DIRECTION('center_axis',(1.,0.,0.));
#10815=DIRECTION('ref_axis',(0.,0.707106781186547,-0.707106781186547));
#10816=DIRECTION('',(0.707106781186532,0.707106781186563,0.));
#10817=DIRECTION('center_axis',(-1.,0.,0.));
#10818=DIRECTION('ref_axis',(0.,0.707106781186548,-0.707106781186548));
#10819=DIRECTION('center_axis',(1.,0.,0.));
#10820=DIRECTION('ref_axis',(0.,0.707106781186547,-0.707106781186547));
#10821=DIRECTION('center_axis',(-0.707106781186555,0.70710678118654,0.));
#10822=DIRECTION('ref_axis',(0.,0.,1.));
#10823=DIRECTION('',(0.70710678118654,0.707106781186555,0.));
#10824=DIRECTION('',(0.,0.,-1.));
#10825=DIRECTION('',(0.,0.,1.));
#10826=DIRECTION('center_axis',(1.,0.,0.));
#10827=DIRECTION('ref_axis',(0.,0.707106781186548,0.707106781186548));
#10828=DIRECTION('',(0.707106781186548,0.,0.707106781186548));
#10829=DIRECTION('center_axis',(-1.,0.,0.));
#10830=DIRECTION('ref_axis',(0.,0.707106781186548,0.707106781186548));
#10831=DIRECTION('center_axis',(1.,0.,0.));
#10832=DIRECTION('ref_axis',(0.,0.707106781186548,0.707106781186548));
#10833=DIRECTION('center_axis',(-0.707106781186532,0.,0.707106781186563));
#10834=DIRECTION('ref_axis',(0.707106781186563,0.,0.707106781186532));
#10835=DIRECTION('',(0.707106781186563,0.,0.707106781186532));
#10836=DIRECTION('',(0.,1.,0.));
#10837=DIRECTION('',(0.,-1.,0.));
#10838=DIRECTION('center_axis',(1.,0.,0.));
#10839=DIRECTION('ref_axis',(0.,-0.707106781186548,0.707106781186548));
#10840=DIRECTION('center_axis',(-1.,0.,0.));
#10841=DIRECTION('ref_axis',(0.,-0.707106781186548,0.707106781186548));
#10842=DIRECTION('center_axis',(1.,0.,0.));
#10843=DIRECTION('ref_axis',(0.,-0.707106781186548,0.707106781186548));
#10844=DIRECTION('center_axis',(1.,0.,0.));
#10845=DIRECTION('ref_axis',(0.,0.707106781186548,0.707106781186548));
#10846=DIRECTION('',(1.,0.,0.));
#10847=DIRECTION('center_axis',(1.,0.,0.));
#10848=DIRECTION('ref_axis',(0.,0.707106781186548,0.707106781186548));
#10849=DIRECTION('',(-1.,0.,0.));
#10850=DIRECTION('center_axis',(0.,0.,1.));
#10851=DIRECTION('ref_axis',(0.,-1.,0.));
#10852=DIRECTION('',(-1.,0.,0.));
#10853=DIRECTION('',(0.,-1.,0.));
#10854=DIRECTION('center_axis',(1.,0.,0.));
#10855=DIRECTION('ref_axis',(0.,-0.707106781186548,0.707106781186548));
#10856=DIRECTION('',(1.,0.,0.));
#10857=DIRECTION('center_axis',(1.,0.,0.));
#10858=DIRECTION('ref_axis',(0.,-0.707106781186548,0.707106781186548));
#10859=DIRECTION('center_axis',(0.,-1.,0.));
#10860=DIRECTION('ref_axis',(0.,0.,-1.));
#10861=DIRECTION('',(-1.,0.,0.));
#10862=DIRECTION('',(0.,0.,-1.));
#10863=DIRECTION('center_axis',(1.,0.,0.));
#10864=DIRECTION('ref_axis',(0.,0.,-1.));
#10865=DIRECTION('center_axis',(1.,0.,0.));
#10866=DIRECTION('ref_axis',(0.,0.,-1.));
#10867=DIRECTION('center_axis',(1.,0.,0.));
#10868=DIRECTION('ref_axis',(0.,0.,-1.));
#10869=DIRECTION('center_axis',(1.,0.,0.));
#10870=DIRECTION('ref_axis',(0.,0.,-1.));
#10871=DIRECTION('center_axis',(1.,0.,0.));
#10872=DIRECTION('ref_axis',(0.,0.,-1.));
#10873=DIRECTION('center_axis',(1.,0.,0.));
#10874=DIRECTION('ref_axis',(0.,0.,-1.));
#10875=DIRECTION('center_axis',(1.,0.,0.));
#10876=DIRECTION('ref_axis',(0.,0.,-1.));
#10877=DIRECTION('center_axis',(-1.,5.71436995156766E-15,0.));
#10878=DIRECTION('ref_axis',(0.,0.,-1.));
#10879=DIRECTION('',(0.382683432365137,1.13142611228768E-16,0.923879532511267));
#10880=DIRECTION('center_axis',(1.,0.,0.));
#10881=DIRECTION('ref_axis',(0.,0.,-1.));
#10882=DIRECTION('center_axis',(1.,0.,0.));
#10883=DIRECTION('ref_axis',(0.,0.,-1.));
#10884=DIRECTION('',(0.,-1.,0.));
#10885=DIRECTION('center_axis',(-1.,0.,0.));
#10886=DIRECTION('ref_axis',(0.,0.707106781186547,-0.707106781186547));
#10887=DIRECTION('',(0.,0.,-1.));
#10888=DIRECTION('center_axis',(-1.,0.,0.));
#10889=DIRECTION('ref_axis',(0.,0.707106781186548,0.707106781186548));
#10890=DIRECTION('',(0.,1.,0.));
#10891=DIRECTION('center_axis',(-1.,0.,0.));
#10892=DIRECTION('ref_axis',(0.,-0.707106781186548,0.707106781186548));
#10893=DIRECTION('',(0.,0.,1.));
#10894=DIRECTION('center_axis',(-1.,0.,0.));
#10895=DIRECTION('ref_axis',(0.,-0.707106781186548,-0.707106781186547));
#10896=DIRECTION('center_axis',(1.,0.,0.));
#10897=DIRECTION('ref_axis',(0.,0.,-1.));
#10898=DIRECTION('center_axis',(-1.,0.,0.));
#10899=DIRECTION('ref_axis',(0.,0.,-1.));
#10900=DIRECTION('center_axis',(1.,0.,0.));
#10901=DIRECTION('ref_axis',(0.,0.,-1.));
#10902=DIRECTION('center_axis',(1.,0.,0.));
#10903=DIRECTION('ref_axis',(0.,0.,-1.));
#10904=DIRECTION('center_axis',(1.,0.,0.));
#10905=DIRECTION('ref_axis',(0.,0.,-1.));
#10906=DIRECTION('',(-0.707106781186545,8.65956056235496E-17,-0.70710678118655));
#10907=DIRECTION('center_axis',(-1.,0.,0.));
#10908=DIRECTION('ref_axis',(0.,0.,-1.));
#10909=DIRECTION('center_axis',(0.707106781186555,0.,-0.70710678118654));
#10910=DIRECTION('ref_axis',(-0.70710678118654,0.,-0.707106781186555));
#10911=DIRECTION('',(0.70710678118654,0.,0.707106781186555));
#10912=DIRECTION('',(-0.70710678118654,0.,-0.707106781186555));
#10913=DIRECTION('',(0.,1.,0.));
#10914=DIRECTION('center_axis',(-1.,0.,0.));
#10915=DIRECTION('ref_axis',(0.,0.707106781186547,-0.707106781186547));
#10916=DIRECTION('center_axis',(1.,0.,0.));
#10917=DIRECTION('ref_axis',(0.,0.707106781186548,-0.707106781186548));
#10918=DIRECTION('',(0.707106781186532,-0.707106781186563,0.));
#10919=DIRECTION('center_axis',(0.707106781186555,0.70710678118654,0.));
#10920=DIRECTION('ref_axis',(0.,0.,-1.));
#10921=DIRECTION('',(0.70710678118654,-0.707106781186555,0.));
#10922=DIRECTION('',(0.,0.,1.));
#10923=DIRECTION('center_axis',(-1.,0.,0.));
#10924=DIRECTION('ref_axis',(0.,0.707106781186548,0.707106781186548));
#10925=DIRECTION('',(0.707106781186548,0.,-0.707106781186548));
#10926=DIRECTION('center_axis',(0.707106781186548,0.,0.707106781186548));
#10927=DIRECTION('ref_axis',(0.707106781186548,0.,-0.707106781186548));
#10928=DIRECTION('',(0.707106781186548,0.,-0.707106781186548));
#10929=DIRECTION('center_axis',(-1.,0.,0.));
#10930=DIRECTION('ref_axis',(0.,-0.707106781186548,0.707106781186548));
#10931=DIRECTION('',(0.707106781186532,0.707106781186563,0.));
#10932=DIRECTION('center_axis',(0.707106781186555,-0.70710678118654,0.));
#10933=DIRECTION('ref_axis',(0.,0.,-1.));
#10934=DIRECTION('',(0.70710678118654,0.707106781186555,0.));
#10935=DIRECTION('center_axis',(-1.,0.,0.));
#10936=DIRECTION('ref_axis',(0.,-0.707106781186548,-0.707106781186547));
#10937=DIRECTION('center_axis',(1.,0.,0.));
#10938=DIRECTION('ref_axis',(0.,-0.707106781186548,-0.707106781186547));
#10939=DIRECTION('center_axis',(0.,1.,0.));
#10940=DIRECTION('ref_axis',(0.,0.,1.));
#10941=DIRECTION('',(1.,0.,0.));
#10942=DIRECTION('center_axis',(1.,0.,0.));
#10943=DIRECTION('ref_axis',(0.,0.707106781186548,-0.707106781186548));
#10944=DIRECTION('',(-1.,0.,0.));
#10945=DIRECTION('center_axis',(0.,0.,-1.));
#10946=DIRECTION('ref_axis',(0.,1.,0.));
#10947=DIRECTION('',(1.,0.,0.));
#10948=DIRECTION('center_axis',(1.,0.,0.));
#10949=DIRECTION('ref_axis',(0.,0.,-1.));
#10950=DIRECTION('center_axis',(-1.,0.,0.));
#10951=DIRECTION('ref_axis',(0.,0.,-1.));
#10952=DIRECTION('',(0.382683432365089,1.1314261122877E-16,0.923879532511287));
#10953=DIRECTION('center_axis',(1.,0.,0.));
#10954=DIRECTION('ref_axis',(0.,0.,-1.));
#10955=DIRECTION('',(-0.707106781186546,8.65956056235495E-17,-0.707106781186548));
#10956=DIRECTION('center_axis',(-1.,0.,0.));
#10957=DIRECTION('ref_axis',(0.,0.,-1.));
#10958=DIRECTION('center_axis',(1.,0.,0.));
#10959=DIRECTION('ref_axis',(0.,0.,-1.));
#10960=DIRECTION('center_axis',(-1.,0.,0.));
#10961=DIRECTION('ref_axis',(0.,0.,-1.));
#10962=DIRECTION('',(0.382683432365089,1.1314261122877E-16,0.923879532511287));
#10963=DIRECTION('center_axis',(1.,0.,0.));
#10964=DIRECTION('ref_axis',(0.,0.,-1.));
#10965=DIRECTION('',(-0.707106781186546,8.65956056235495E-17,-0.707106781186548));
#10966=DIRECTION('center_axis',(-1.,0.,0.));
#10967=DIRECTION('ref_axis',(0.,0.,-1.));
#10968=DIRECTION('center_axis',(1.,0.,0.));
#10969=DIRECTION('ref_axis',(0.,0.,-1.));
#10970=DIRECTION('center_axis',(-1.,5.71436995156766E-15,0.));
#10971=DIRECTION('ref_axis',(0.,0.,-1.));
#10972=DIRECTION('',(0.382683432365137,1.13142611228768E-16,0.923879532511267));
#10973=DIRECTION('center_axis',(1.,0.,0.));
#10974=DIRECTION('ref_axis',(0.,0.,-1.));
#10975=DIRECTION('',(-0.707106781186545,8.65956056235496E-17,-0.70710678118655));
#10976=DIRECTION('center_axis',(-1.,0.,0.));
#10977=DIRECTION('ref_axis',(0.,0.,-1.));
#10978=DIRECTION('center_axis',(-1.,0.,0.));
#10979=DIRECTION('ref_axis',(0.,0.,-1.));
#10980=DIRECTION('',(-1.,0.,0.));
#10981=DIRECTION('center_axis',(-1.,0.,0.));
#10982=DIRECTION('ref_axis',(0.,0.,-1.));
#10983=DIRECTION('',(-1.,0.,0.));
#10984=DIRECTION('center_axis',(-1.,0.,0.));
#10985=DIRECTION('ref_axis',(0.,0.,-1.));
#10986=DIRECTION('',(-1.,0.,0.));
#10987=DIRECTION('center_axis',(-1.,0.,0.));
#10988=DIRECTION('ref_axis',(0.,0.,-1.));
#10989=DIRECTION('',(-1.,0.,0.));
#10990=DIRECTION('center_axis',(-1.,0.,0.));
#10991=DIRECTION('ref_axis',(0.,0.,-1.));
#10992=DIRECTION('',(-1.,0.,0.));
#10993=DIRECTION('center_axis',(1.,0.,0.));
#10994=DIRECTION('ref_axis',(0.,-0.707106781186548,-0.707106781186547));
#10995=DIRECTION('axis',(0.,0.,1.));
#10996=DIRECTION('refdir',(1.,0.,0.));
#10997=DIRECTION('center_axis',(-1.,0.,0.));
#10998=DIRECTION('ref_axis',(0.,0.,-1.));
#10999=DIRECTION('center_axis',(-1.,0.,0.));
#11000=DIRECTION('ref_axis',(0.,0.,-1.));
#11001=DIRECTION('',(0.707106781186549,-8.65956056235492E-17,-0.707106781186546));
#11002=DIRECTION('center_axis',(1.,0.,0.));
#11003=DIRECTION('ref_axis',(0.,0.,-1.));
#11004=DIRECTION('center_axis',(1.,0.,0.));
#11005=DIRECTION('ref_axis',(0.,0.,-1.));
#11006=DIRECTION('',(0.,-0.707106781186547,-0.707106781186548));
#11007=DIRECTION('',(0.,-0.923879532511285,-0.382683432365095));
#11008=DIRECTION('',(0.,-1.,0.));
#11009=DIRECTION('',(0.,-0.707106781186548,0.707106781186548));
#11010=DIRECTION('',(0.,0.,1.));
#11011=DIRECTION('',(0.,0.707106781186542,0.707106781186553));
#11012=DIRECTION('',(0.,1.,0.));
#11013=DIRECTION('',(0.,0.,1.));
#11014=DIRECTION('',(0.,-1.,0.));
#11015=DIRECTION('',(0.,-0.707106781186553,0.707106781186542));
#11016=DIRECTION('',(0.,0.,1.));
#11017=DIRECTION('',(0.,0.707106781186548,0.707106781186547));
#11018=DIRECTION('',(0.,1.,0.));
#11019=DIRECTION('',(0.,0.70710678118655,-0.707106781186545));
#11020=DIRECTION('',(0.,0.,-1.));
#11021=DIRECTION('',(0.,1.,0.));
#11022=DIRECTION('',(0.,0.,1.));
#11023=DIRECTION('',(0.,0.707106781186546,0.707106781186549));
#11024=DIRECTION('',(0.,1.,0.));
#11025=DIRECTION('',(0.,0.923879532511286,-0.382683432365093));
#11026=DIRECTION('',(0.,0.707106781186548,-0.707106781186548));
#11027=DIRECTION('',(0.,0.,-1.));
#11028=DIRECTION('center_axis',(1.,0.,0.));
#11029=DIRECTION('ref_axis',(0.,0.,-1.));
#11030=DIRECTION('',(0.,0.,-1.));
#11031=DIRECTION('center_axis',(-1.,0.,0.));
#11032=DIRECTION('ref_axis',(0.,0.,-1.));
#11033=DIRECTION('center_axis',(1.,0.,0.));
#11034=DIRECTION('ref_axis',(0.,0.,-1.));
#11035=DIRECTION('',(1.,0.,0.));
#11036=DIRECTION('center_axis',(1.,0.,0.));
#11037=DIRECTION('ref_axis',(0.,0.,-1.));
#11038=DIRECTION('center_axis',(-1.,0.,0.));
#11039=DIRECTION('ref_axis',(0.,0.,-1.));
#11040=DIRECTION('',(0.707106781186549,-8.65956056235492E-17,-0.707106781186546));
#11041=DIRECTION('center_axis',(1.,0.,0.));
#11042=DIRECTION('ref_axis',(0.,0.,-1.));
#11043=DIRECTION('center_axis',(1.,0.,0.));
#11044=DIRECTION('ref_axis',(0.,0.,-1.));
#11045=DIRECTION('',(1.,0.,0.));
#11046=DIRECTION('center_axis',(1.,0.,0.));
#11047=DIRECTION('ref_axis',(0.,0.,-1.));
#11048=DIRECTION('center_axis',(0.,-0.555570233019621,0.831469612302533));
#11049=DIRECTION('ref_axis',(1.,0.,0.));
#11050=DIRECTION('',(-0.191480453955336,0.816084453438868,0.545290198525925));
#11051=DIRECTION('',(-1.,0.,0.));
#11052=DIRECTION('',(-0.19148045395534,-0.816084453438867,-0.545290198525924));
#11053=DIRECTION('',(0.191480453955301,-0.816084453438874,-0.545290198525928));
#11054=DIRECTION('',(1.,0.,0.));
#11055=DIRECTION('',(0.191480453955304,0.816084453438873,0.545290198525928));
#11056=DIRECTION('center_axis',(0.,-0.382683432365095,0.923879532511285));
#11057=DIRECTION('ref_axis',(1.,0.,0.));
#11058=DIRECTION('',(0.,-0.923879532511285,-0.382683432365095));
#11059=DIRECTION('',(1.,0.,0.));
#11060=DIRECTION('',(0.,0.923879532511285,0.382683432365095));
#11061=DIRECTION('center_axis',(0.707106781186551,-0.270598050073101,0.653281482438184));
#11062=DIRECTION('ref_axis',(0.678598344545843,0.,-0.734509555267759));
#11063=DIRECTION('',(-0.700214507282553,-0.396639656760255,0.593613196009116));
#11064=DIRECTION('',(0.,0.923879532511285,0.382683432365095));
#11065=DIRECTION('',(-0.700214507282553,-0.139281325317155,0.700214507282553));
#11066=DIRECTION('',(0.191480453955321,0.962637248139779,0.191480453955329));
#11067=DIRECTION('center_axis',(0.707106781186544,-0.500000000000003,0.500000000000002));
#11068=DIRECTION('ref_axis',(0.57735026918963,0.,-0.816496580927723));
#11069=DIRECTION('',(0.,-0.707106781186547,-0.707106781186548));
#11070=DIRECTION('',(0.653281482438189,0.191341716182535,-0.732537816328744));
#11071=DIRECTION('',(0.,0.707106781186547,0.707106781186548));
#11072=DIRECTION('center_axis',(0.,-0.195090322016134,0.980785280403229));
#11073=DIRECTION('ref_axis',(1.,0.,0.));
#11074=DIRECTION('',(0.191480453955325,-0.962637248139778,-0.191480453955328));
#11075=DIRECTION('',(-0.191480453955328,0.962637248139777,0.191480453955328));
#11076=DIRECTION('',(-1.,0.,0.));
#11077=DIRECTION('',(-0.191480453955332,-0.962637248139776,-0.191480453955328));
#11078=DIRECTION('center_axis',(-0.707106781186543,-0.270598050073104,0.653281482438191));
#11079=DIRECTION('ref_axis',(0.678598344545851,0.,0.734509555267752));
#11080=DIRECTION('',(0.700214507282561,-0.139281325317153,0.700214507282546));
#11081=DIRECTION('',(-0.700214507282555,0.396639656760308,-0.59361319600908));
#11082=DIRECTION('center_axis',(-0.70710678118654,0.,0.707106781186555));
#11083=DIRECTION('ref_axis',(0.707106781186555,0.,0.70710678118654));
#11084=DIRECTION('',(0.,1.,0.));
#11085=DIRECTION('',(0.678598344545856,0.281084637714812,0.678598344545841));
#11086=DIRECTION('center_axis',(1.,0.,0.));
#11087=DIRECTION('ref_axis',(0.,0.,-1.));
#11088=DIRECTION('center_axis',(1.,0.,0.));
#11089=DIRECTION('ref_axis',(0.,0.,-1.));
#11090=DIRECTION('',(-0.707106781186554,8.65956056235486E-17,-0.707106781186541));
#11091=DIRECTION('center_axis',(-1.,0.,0.));
#11092=DIRECTION('ref_axis',(0.,0.,-1.));
#11093=DIRECTION('center_axis',(1.,0.,0.));
#11094=DIRECTION('ref_axis',(0.,0.,-1.));
#11095=DIRECTION('',(0.,0.,1.));
#11096=DIRECTION('center_axis',(-1.,0.,0.));
#11097=DIRECTION('ref_axis',(0.,0.,-1.));
#11098=DIRECTION('',(0.,0.,1.));
#11099=DIRECTION('',(0.,-0.707106781186548,0.707106781186548));
#11100=DIRECTION('',(0.,-0.923879532511286,0.382683432365093));
#11101=DIRECTION('',(0.,-1.,0.));
#11102=DIRECTION('',(0.,-0.707106781186546,-0.707106781186549));
#11103=DIRECTION('',(0.,0.,-1.));
#11104=DIRECTION('',(0.,-1.,0.));
#11105=DIRECTION('',(0.,0.,1.));
#11106=DIRECTION('',(0.,-0.70710678118655,0.707106781186545));
#11107=DIRECTION('',(0.,-1.,0.));
#11108=DIRECTION('',(0.,-0.707106781186548,-0.707106781186547));
#11109=DIRECTION('',(0.,0.,-1.));
#11110=DIRECTION('',(0.,0.707106781186553,-0.707106781186542));
#11111=DIRECTION('',(0.,1.,0.));
#11112=DIRECTION('',(0.,0.,-1.));
#11113=DIRECTION('',(0.,-1.,0.));
#11114=DIRECTION('',(0.,-0.707106781186542,-0.707106781186553));
#11115=DIRECTION('',(0.,0.,-1.));
#11116=DIRECTION('',(0.,0.707106781186548,-0.707106781186548));
#11117=DIRECTION('',(0.,1.,0.));
#11118=DIRECTION('center_axis',(1.,0.,0.));
#11119=DIRECTION('ref_axis',(0.,0.,-1.));
#11120=DIRECTION('center_axis',(-1.,0.,0.));
#11121=DIRECTION('ref_axis',(0.,0.,-1.));
#11122=DIRECTION('',(-1.,0.,0.));
#11123=DIRECTION('center_axis',(-1.,0.,0.));
#11124=DIRECTION('ref_axis',(0.,0.,-1.));
#11125=DIRECTION('center_axis',(1.,0.,0.));
#11126=DIRECTION('ref_axis',(0.,0.,-1.));
#11127=DIRECTION('',(-0.707106781186554,8.65956056235486E-17,-0.707106781186541));
#11128=DIRECTION('center_axis',(-1.,0.,0.));
#11129=DIRECTION('ref_axis',(0.,0.,-1.));
#11130=DIRECTION('center_axis',(-1.,0.,0.));
#11131=DIRECTION('ref_axis',(0.,0.,-1.));
#11132=DIRECTION('',(-1.,0.,0.));
#11133=DIRECTION('center_axis',(-1.,0.,0.));
#11134=DIRECTION('ref_axis',(0.,0.,-1.));
#11135=DIRECTION('center_axis',(-0.57330218625602,-0.756975158957756,0.313549377219837));
#11136=DIRECTION('ref_axis',(0.479841491130337,0.,0.877355197961359));
#11137=DIRECTION('',(0.,-0.382683432365094,-0.923879532511285));
#11138=DIRECTION('',(0.653281482438184,-0.191341716182538,0.732537816328748));
#11139=DIRECTION('',(-0.653281482438192,0.653281482438192,0.382683432365078));
#11140=DIRECTION('center_axis',(-0.707106781186549,-0.499999999999999,0.499999999999999));
#11141=DIRECTION('ref_axis',(0.577350269189624,0.,0.816496580927727));
#11142=DIRECTION('',(0.,0.707106781186547,0.707106781186548));
#11143=DIRECTION('center_axis',(-0.707106781186547,-0.707106781186548,0.));
#11144=DIRECTION('ref_axis',(0.,0.,1.));
#11145=DIRECTION('center_axis',(0.707106781186547,0.707106781186548,0.));
#11146=DIRECTION('ref_axis',(-0.707106781186548,0.707106781186547,0.));
#11147=DIRECTION('',(0.,0.,1.));
#11148=DIRECTION('center_axis',(0.573302186256015,-0.75697515895776,0.313549377219838));
#11149=DIRECTION('ref_axis',(0.479841491130341,0.,-0.877355197961356));
#11150=DIRECTION('',(0.,0.382683432365094,0.923879532511285));
#11151=DIRECTION('',(-0.653281482438197,-0.653281482438188,-0.382683432365075));
#11152=DIRECTION('center_axis',(0.,-0.923879532511285,0.382683432365094));
#11153=DIRECTION('ref_axis',(0.,-0.382683432365094,-0.923879532511285));
#11154=DIRECTION('',(-1.,0.,0.));
#11155=DIRECTION('',(1.,0.,0.));
#11156=DIRECTION('center_axis',(0.707106781186542,-0.707106781186553,0.));
#11157=DIRECTION('ref_axis',(0.,0.,-1.));
#11158=DIRECTION('center_axis',(-0.707106781186542,0.707106781186553,0.));
#11159=DIRECTION('ref_axis',(0.707106781186553,0.707106781186542,0.));
#11160=DIRECTION('',(0.,0.,-1.));
#11161=DIRECTION('center_axis',(0.,-0.707106781186548,0.707106781186547));
#11162=DIRECTION('ref_axis',(0.,-0.707106781186547,-0.707106781186548));
#11163=DIRECTION('center_axis',(-0.573302186256016,-0.756975158957761,-0.313549377219833));
#11164=DIRECTION('ref_axis',(-0.479841491130335,0.,0.87735519796136));
#11165=DIRECTION('',(0.653281482438192,-0.653281482438192,0.382683432365078));
#11166=DIRECTION('',(-0.653281482438188,0.191341716182541,0.732537816328743));
#11167=DIRECTION('',(0.,0.382683432365089,-0.923879532511287));
#11168=DIRECTION('center_axis',(-0.707106781186547,-0.5,-0.5));
#11169=DIRECTION('ref_axis',(-0.577350269189626,0.,0.816496580927726));
#11170=DIRECTION('',(0.357406744336591,-0.862856209461017,0.357406744336596));
#11171=DIRECTION('',(0.,-0.707106781186548,0.707106781186548));
#11172=DIRECTION('',(0.700214507282551,-0.396639656760267,-0.593613196009111));
#11173=DIRECTION('center_axis',(0.573302186256013,-0.756975158957763,-0.313549377219834));
#11174=DIRECTION('ref_axis',(-0.479841491130337,0.,-0.877355197961358));
#11175=DIRECTION('',(0.653281482438194,0.653281482438185,-0.382683432365085));
#11176=DIRECTION('',(0.,-0.382683432365089,0.923879532511287));
#11177=DIRECTION('',(-0.653281482438194,-0.191341716182545,-0.732537816328737));
#11178=DIRECTION('center_axis',(0.,-0.923879532511287,-0.382683432365089));
#11179=DIRECTION('ref_axis',(0.,0.382683432365089,-0.923879532511287));
#11180=DIRECTION('',(-1.,0.,0.));
#11181=DIRECTION('',(1.,0.,0.));
#11182=DIRECTION('center_axis',(0.707106781186542,-0.500000000000004,-0.500000000000004));
#11183=DIRECTION('ref_axis',(-0.577350269189631,0.,-0.816496580927722));
#11184=DIRECTION('',(0.70021450728255,0.396639656760214,0.593613196009148));
#11185=DIRECTION('',(0.,0.707106781186548,-0.707106781186548));
#11186=DIRECTION('',(0.357406744336595,0.862856209461015,-0.357406744336596));
#11187=DIRECTION('center_axis',(0.707106781186542,-0.707106781186553,0.));
#11188=DIRECTION('ref_axis',(0.,0.,-1.));
#11189=DIRECTION('center_axis',(-0.707106781186542,0.707106781186553,0.));
#11190=DIRECTION('ref_axis',(0.707106781186553,0.707106781186542,0.));
#11191=DIRECTION('',(0.,0.,-1.));
#11192=DIRECTION('center_axis',(-0.707106781186547,-0.707106781186548,0.));
#11193=DIRECTION('ref_axis',(0.,0.,1.));
#11194=DIRECTION('center_axis',(0.707106781186547,0.707106781186548,0.));
#11195=DIRECTION('ref_axis',(-0.707106781186548,0.707106781186547,0.));
#11196=DIRECTION('',(0.,0.,1.));
#11197=DIRECTION('center_axis',(0.,-1.,0.));
#11198=DIRECTION('ref_axis',(0.,0.,-1.));
#11199=DIRECTION('',(-1.,0.,0.));
#11200=DIRECTION('center_axis',(0.,1.,0.));
#11201=DIRECTION('ref_axis',(1.,0.,0.));
#11202=DIRECTION('center_axis',(0.,1.,0.));
#11203=DIRECTION('ref_axis',(1.,0.,0.));
#11204=DIRECTION('center_axis',(0.,1.,0.));
#11205=DIRECTION('ref_axis',(1.,0.,0.));
#11206=DIRECTION('center_axis',(1.,0.,0.));
#11207=DIRECTION('ref_axis',(0.,0.,-1.));
#11208=DIRECTION('',(1.,0.,0.));
#11209=DIRECTION('center_axis',(0.707106781186559,-0.270598050073096,-0.653281482438177));
#11210=DIRECTION('ref_axis',(-0.678598344545835,0.,-0.734509555267767));
#11211=DIRECTION('',(0.,0.923879532511286,-0.382683432365093));
#11212=DIRECTION('',(-0.700214507282542,-0.139281325317168,-0.700214507282561));
#11213=DIRECTION('center_axis',(0.707106781186555,0.,0.70710678118654));
#11214=DIRECTION('ref_axis',(0.70710678118654,0.,-0.707106781186555));
#11215=DIRECTION('',(0.,-1.,0.));
#11216=DIRECTION('',(0.577350269189617,-0.57735026918963,-0.57735026918963));
#11217=DIRECTION('',(-0.678598344545838,0.281084637714811,0.67859834454586));
#11218=DIRECTION('center_axis',(0.707106781186548,0.,0.707106781186548));
#11219=DIRECTION('ref_axis',(0.707106781186548,0.,-0.707106781186548));
#11220=DIRECTION('',(-0.678598344545848,0.281084637714815,0.678598344545848));
#11221=DIRECTION('',(0.,-1.,0.));
#11222=DIRECTION('center_axis',(0.70710678118654,0.500000000000005,0.500000000000005));
#11223=DIRECTION('ref_axis',(0.577350269189634,0.,-0.81649658092772));
#11224=DIRECTION('',(-0.678598344545841,0.678598344545856,0.281084637714812));
#11225=DIRECTION('',(0.,-0.707106781186548,0.707106781186548));
#11226=DIRECTION('center_axis',(0.707106781186555,0.70710678118654,0.));
#11227=DIRECTION('ref_axis',(0.,0.,-1.));
#11228=DIRECTION('',(-0.678598344545839,0.678598344545846,-0.281084637714841));
#11229=DIRECTION('',(0.,0.,1.));
#11230=DIRECTION('center_axis',(0.707106781186559,0.499999999999995,-0.499999999999988));
#11231=DIRECTION('ref_axis',(-0.57735026918961,0.,-0.816496580927737));
#11232=DIRECTION('',(0.,0.707106781186542,0.707106781186553));
#11233=DIRECTION('',(-0.678598344545837,0.281084637714833,-0.678598344545852));
#11234=DIRECTION('center_axis',(0.707106781186555,0.,-0.70710678118654));
#11235=DIRECTION('ref_axis',(-0.70710678118654,0.,-0.707106781186555));
#11236=DIRECTION('',(0.,1.,0.));
#11237=DIRECTION('',(-0.577350269189617,0.57735026918963,-0.57735026918963));
#11238=DIRECTION('center_axis',(0.707106781186555,0.70710678118654,0.));
#11239=DIRECTION('ref_axis',(0.,0.,-1.));
#11240=DIRECTION('',(0.,0.,1.));
#11241=DIRECTION('center_axis',(0.707106781186554,0.499999999999992,0.499999999999999));
#11242=DIRECTION('ref_axis',(0.577350269189622,0.,-0.816496580927729));
#11243=DIRECTION('',(0.,-0.707106781186553,0.707106781186542));
#11244=DIRECTION('',(-0.67859834454584,0.678598344545855,0.281084637714819));
#11245=DIRECTION('center_axis',(0.707106781186555,0.70710678118654,0.));
#11246=DIRECTION('ref_axis',(0.,0.,-1.));
#11247=DIRECTION('',(0.,0.,1.));
#11248=DIRECTION('',(-0.678598344545827,0.678598344545842,-0.281084637714881));
#11249=DIRECTION('center_axis',(0.707106781186577,0.499999999999979,-0.49999999999998));
#11250=DIRECTION('ref_axis',(-0.577350269189594,0.,-0.816496580927748));
#11251=DIRECTION('',(0.,0.707106781186548,0.707106781186547));
#11252=DIRECTION('',(-0.678598344545828,0.281084637714875,-0.678598344545843));
#11253=DIRECTION('center_axis',(0.707106781186555,0.,-0.70710678118654));
#11254=DIRECTION('ref_axis',(-0.70710678118654,0.,-0.707106781186555));
#11255=DIRECTION('',(0.,1.,0.));
#11256=DIRECTION('',(-0.67859834454584,-0.281084637714819,-0.678598344545855));
#11257=DIRECTION('center_axis',(0.707106781186555,-0.499999999999993,-0.499999999999997));
#11258=DIRECTION('ref_axis',(-0.577350269189619,0.,-0.816496580927731));
#11259=DIRECTION('',(0.,0.70710678118655,-0.707106781186545));
#11260=DIRECTION('',(-0.678598344545838,-0.678598344545853,-0.281084637714827));
#11261=DIRECTION('center_axis',(0.707106781186555,-0.70710678118654,0.));
#11262=DIRECTION('ref_axis',(0.,0.,-1.));
#11263=DIRECTION('',(0.,0.,-1.));
#11264=DIRECTION('',(-0.577350269189617,-0.57735026918963,-0.57735026918963));
#11265=DIRECTION('center_axis',(0.707106781186555,0.,-0.70710678118654));
#11266=DIRECTION('ref_axis',(-0.70710678118654,0.,-0.707106781186555));
#11267=DIRECTION('',(0.,1.,0.));
#11268=DIRECTION('',(-0.577350269189617,0.57735026918963,-0.57735026918963));
#11269=DIRECTION('center_axis',(0.707106781186555,0.70710678118654,0.));
#11270=DIRECTION('ref_axis',(0.,0.,-1.));
#11271=DIRECTION('',(0.,0.,1.));
#11272=DIRECTION('',(-0.678598344545838,0.678598344545853,-0.281084637714826));
#11273=DIRECTION('center_axis',(0.707106781186555,0.499999999999996,-0.499999999999993));
#11274=DIRECTION('ref_axis',(-0.577350269189616,0.,-0.816496580927733));
#11275=DIRECTION('',(0.,0.707106781186546,0.707106781186549));
#11276=DIRECTION('',(-0.678598344545837,0.281084637714826,-0.678598344545855));
#11277=DIRECTION('center_axis',(0.707106781186557,0.,-0.707106781186538));
#11278=DIRECTION('ref_axis',(-0.707106781186538,0.,-0.707106781186557));
#11279=DIRECTION('',(0.,1.,0.));
#11280=DIRECTION('center_axis',(0.,-0.707106781186545,-0.70710678118655));
#11281=DIRECTION('ref_axis',(-1.,0.,0.));
#11282=DIRECTION('',(-1.,0.,0.));
#11283=DIRECTION('',(0.,-0.70710678118655,0.707106781186545));
#11284=DIRECTION('',(1.,0.,0.));
#11285=DIRECTION('center_axis',(0.,-1.,0.));
#11286=DIRECTION('ref_axis',(0.,0.,-1.));
#11287=DIRECTION('',(1.,0.,0.));
#11288=DIRECTION('',(0.,0.,1.));
#11289=DIRECTION('center_axis',(0.,0.,-1.));
#11290=DIRECTION('ref_axis',(0.,1.,0.));
#11291=DIRECTION('',(1.,0.,0.));
#11292=DIRECTION('',(0.,-1.,0.));
#11293=DIRECTION('center_axis',(0.,1.,0.));
#11294=DIRECTION('ref_axis',(0.,0.,1.));
#11295=DIRECTION('',(1.,0.,0.));
#11296=DIRECTION('',(0.,0.,-1.));
#11297=DIRECTION('center_axis',(0.,0.707106781186549,-0.707106781186546));
#11298=DIRECTION('ref_axis',(-1.,0.,0.));
#11299=DIRECTION('',(-1.,0.,0.));
#11300=DIRECTION('',(0.,-0.707106781186546,-0.707106781186549));
#11301=DIRECTION('center_axis',(0.,0.,-1.));
#11302=DIRECTION('ref_axis',(0.,1.,0.));
#11303=DIRECTION('',(1.,0.,0.));
#11304=DIRECTION('',(0.,-1.,0.));
#11305=DIRECTION('center_axis',(0.,-0.382683432365093,-0.923879532511286));
#11306=DIRECTION('ref_axis',(-1.,0.,0.));
#11307=DIRECTION('',(0.,-0.923879532511286,0.382683432365093));
#11308=DIRECTION('',(-1.,0.,0.));
#11309=DIRECTION('center_axis',(0.,-0.707106781186548,-0.707106781186548));
#11310=DIRECTION('ref_axis',(0.,0.707106781186548,-0.707106781186548));
#11311=DIRECTION('center_axis',(-0.707106781186551,-0.270598050073099,-0.653281482438184));
#11312=DIRECTION('ref_axis',(-0.678598344545843,0.,0.73450955526776));
#11313=DIRECTION('',(0.70021450728255,-0.13928132531717,-0.700214507282553));
#11314=DIRECTION('center_axis',(-0.707106781186549,0.,-0.707106781186546));
#11315=DIRECTION('ref_axis',(-0.707106781186546,0.,0.707106781186549));
#11316=DIRECTION('',(0.678598344545846,0.281084637714823,-0.678598344545847));
#11317=DIRECTION('center_axis',(-0.707106781186548,0.500000000000001,-0.499999999999999));
#11318=DIRECTION('ref_axis',(-0.577350269189625,0.,0.816496580927727));
#11319=DIRECTION('',(0.678598344545846,0.678598344545847,-0.281084637714823));
#11320=DIRECTION('center_axis',(-0.707106781186548,0.707106781186547,0.));
#11321=DIRECTION('ref_axis',(0.,0.,1.));
#11322=DIRECTION('',(0.577350269189626,0.577350269189626,-0.577350269189626));
#11323=DIRECTION('center_axis',(-0.707106781186548,0.,-0.707106781186547));
#11324=DIRECTION('ref_axis',(-0.707106781186547,0.,0.707106781186548));
#11325=DIRECTION('',(0.577350269189626,-0.577350269189626,-0.577350269189626));
#11326=DIRECTION('center_axis',(-0.707106781186548,-0.707106781186547,0.));
#11327=DIRECTION('ref_axis',(0.,0.,1.));
#11328=DIRECTION('',(0.678598344545847,-0.678598344545847,-0.281084637714821));
#11329=DIRECTION('center_axis',(-0.707106781186548,-0.499999999999998,-0.500000000000002));
#11330=DIRECTION('ref_axis',(-0.577350269189627,0.,0.816496580927725));
#11331=DIRECTION('',(0.678598344545848,-0.281084637714816,-0.678598344545848));
#11332=DIRECTION('center_axis',(-0.707106781186548,0.,-0.707106781186547));
#11333=DIRECTION('ref_axis',(-0.707106781186547,0.,0.707106781186548));
#11334=DIRECTION('',(0.678598344545835,0.281084637714872,-0.678598344545838));
#11335=DIRECTION('',(0.,-1.,0.));
#11336=DIRECTION('center_axis',(-0.707106781186569,0.499999999999984,-0.499999999999985));
#11337=DIRECTION('ref_axis',(-0.577350269189602,0.,0.816496580927743));
#11338=DIRECTION('',(0.678598344545836,0.678598344545836,-0.281084637714873));
#11339=DIRECTION('',(0.,-0.707106781186548,-0.707106781186547));
#11340=DIRECTION('center_axis',(-0.707106781186548,0.707106781186547,0.));
#11341=DIRECTION('ref_axis',(0.,0.,1.));
#11342=DIRECTION('',(0.678598344545846,0.678598344545847,0.281084637714823));
#11343=DIRECTION('',(0.,0.,-1.));
#11344=DIRECTION('center_axis',(-0.707106781186546,0.499999999999997,0.500000000000005));
#11345=DIRECTION('ref_axis',(0.57735026918963,0.,0.816496580927723));
#11346=DIRECTION('',(0.678598344545848,0.281084637714816,0.678598344545848));
#11347=DIRECTION('',(0.,0.707106781186553,-0.707106781186542));
#11348=DIRECTION('center_axis',(-0.707106781186548,0.,0.707106781186547));
#11349=DIRECTION('ref_axis',(0.707106781186547,0.,0.707106781186548));
#11350=DIRECTION('',(0.577350269189626,0.577350269189626,0.577350269189626));
#11351=DIRECTION('',(0.,1.,0.));
#11352=DIRECTION('center_axis',(-0.707106781186548,0.,-0.707106781186547));
#11353=DIRECTION('ref_axis',(-0.707106781186547,0.,0.707106781186548));
#11354=DIRECTION('',(0.678598344545845,0.28108463771483,-0.678598344545845));
#11355=DIRECTION('',(0.,-1.,0.));
#11356=DIRECTION('',(-0.577350269189626,-0.577350269189626,0.577350269189626));
#11357=DIRECTION('center_axis',(-0.707106781186552,0.500000000000001,-0.499999999999993));
#11358=DIRECTION('ref_axis',(-0.577350269189618,0.,0.816496580927731));
#11359=DIRECTION('',(0.,-0.707106781186542,-0.707106781186553));
#11360=DIRECTION('',(0.678598344545846,0.678598344545847,-0.281084637714823));
#11361=DIRECTION('center_axis',(-0.707106781186548,0.707106781186547,0.));
#11362=DIRECTION('ref_axis',(0.,0.,1.));
#11363=DIRECTION('',(0.,0.,-1.));
#11364=DIRECTION('',(0.678598344545853,0.678598344545845,0.281084637714811));
#11365=DIRECTION('center_axis',(-0.707106781186548,0.707106781186547,0.));
#11366=DIRECTION('ref_axis',(0.,0.,1.));
#11367=DIRECTION('',(0.,0.,-1.));
#11368=DIRECTION('center_axis',(-0.707106781186532,0.500000000000011,0.500000000000011));
#11369=DIRECTION('ref_axis',(0.577350269189642,0.,0.816496580927714));
#11370=DIRECTION('',(0.,0.707106781186548,-0.707106781186548));
#11371=DIRECTION('center_axis',(0.,0.,-1.));
#11372=DIRECTION('ref_axis',(0.,1.,0.));
#11373=DIRECTION('',(-1.,0.,0.));
#11374=DIRECTION('center_axis',(0.,0.707106781186547,-0.707106781186548));
#11375=DIRECTION('ref_axis',(-1.,0.,0.));
#11376=DIRECTION('',(1.,0.,0.));
#11377=DIRECTION('center_axis',(0.,1.,0.));
#11378=DIRECTION('ref_axis',(0.,0.,1.));
#11379=DIRECTION('',(-1.,0.,0.));
#11380=DIRECTION('center_axis',(0.,-1.,0.));
#11381=DIRECTION('ref_axis',(1.,0.,0.));
#11382=DIRECTION('center_axis',(0.,-1.,0.));
#11383=DIRECTION('ref_axis',(1.,0.,0.));
#11384=DIRECTION('center_axis',(0.,-1.,0.));
#11385=DIRECTION('ref_axis',(1.,0.,0.));
#11386=DIRECTION('center_axis',(0.,0.707106781186542,0.707106781186553));
#11387=DIRECTION('ref_axis',(1.,0.,0.));
#11388=DIRECTION('',(1.,0.,0.));
#11389=DIRECTION('center_axis',(0.,0.,-1.));
#11390=DIRECTION('ref_axis',(0.,1.,0.));
#11391=DIRECTION('',(1.,0.,0.));
#11392=DIRECTION('center_axis',(0.,-1.,0.));
#11393=DIRECTION('ref_axis',(0.,0.,-1.));
#11394=DIRECTION('',(1.,0.,0.));
#11395=DIRECTION('center_axis',(0.,0.,1.));
#11396=DIRECTION('ref_axis',(0.,-1.,0.));
#11397=DIRECTION('',(-1.,0.,0.));
#11398=DIRECTION('center_axis',(0.,0.707106781186553,-0.707106781186542));
#11399=DIRECTION('ref_axis',(-1.,0.,0.));
#11400=DIRECTION('',(1.,0.,0.));
#11401=DIRECTION('center_axis',(0.,1.,0.));
#11402=DIRECTION('ref_axis',(0.,0.,1.));
#11403=DIRECTION('',(-1.,0.,0.));
#11404=DIRECTION('center_axis',(0.,0.707106781186548,0.707106781186548));
#11405=DIRECTION('ref_axis',(1.,0.,0.));
#11406=DIRECTION('',(1.,0.,0.));
#11407=DIRECTION('center_axis',(0.,0.,1.));
#11408=DIRECTION('ref_axis',(0.,-1.,0.));
#11409=DIRECTION('center_axis',(1.,0.,0.));
#11410=DIRECTION('ref_axis',(0.,0.,-1.));
#11411=DIRECTION('center_axis',(1.,0.,0.));
#11412=DIRECTION('ref_axis',(0.,0.,-1.));
#11413=DIRECTION('center_axis',(1.,0.,0.));
#11414=DIRECTION('ref_axis',(0.,0.,-1.));
#11415=DIRECTION('center_axis',(1.,0.,0.));
#11416=DIRECTION('ref_axis',(0.,0.,-1.));
#11417=DIRECTION('center_axis',(0.,-1.,0.));
#11418=DIRECTION('ref_axis',(1.,0.,0.));
#11419=DIRECTION('',(0.,-1.,0.));
#11420=DIRECTION('center_axis',(0.,-1.,0.));
#11421=DIRECTION('ref_axis',(1.,0.,0.));
#11422=DIRECTION('',(0.,-1.,0.));
#11423=DIRECTION('center_axis',(0.,-1.,0.));
#11424=DIRECTION('ref_axis',(1.,0.,0.));
#11425=DIRECTION('',(0.,-1.,0.));
#11426=DIRECTION('center_axis',(0.,-1.,0.));
#11427=DIRECTION('ref_axis',(0.,0.,-1.));
#11428=DIRECTION('axis',(0.,0.,1.));
#11429=DIRECTION('refdir',(1.,0.,0.));
#11430=DIRECTION('center_axis',(-1.,0.,0.));
#11431=DIRECTION('ref_axis',(0.,0.,1.));
#11432=DIRECTION('center_axis',(1.,0.,0.));
#11433=DIRECTION('ref_axis',(0.,0.,-1.));
#11434=DIRECTION('center_axis',(1.,0.,0.));
#11435=DIRECTION('ref_axis',(0.,1.,0.));
#11436=DIRECTION('center_axis',(1.,0.,0.));
#11437=DIRECTION('ref_axis',(0.,0.,-1.));
#11438=DIRECTION('',(-0.707106781186547,0.707106781186548,8.65956056235494E-17));
#11439=DIRECTION('center_axis',(1.,0.,0.));
#11440=DIRECTION('ref_axis',(0.,1.,0.));
#11441=DIRECTION('center_axis',(1.,0.,0.));
#11442=DIRECTION('ref_axis',(0.,0.,-1.));
#11443=DIRECTION('',(-1.,0.,0.));
#11444=DIRECTION('center_axis',(-1.,0.,0.));
#11445=DIRECTION('ref_axis',(0.,1.,0.));
#11446=DIRECTION('center_axis',(1.,0.,0.));
#11447=DIRECTION('ref_axis',(0.,0.,-1.));
#11448=DIRECTION('',(-0.707106781186552,-0.707106781186543,-8.65956056235488E-17));
#11449=DIRECTION('center_axis',(1.,0.,0.));
#11450=DIRECTION('ref_axis',(0.,0.,-1.));
#11451=DIRECTION('axis',(0.,0.,1.));
#11452=DIRECTION('refdir',(1.,0.,0.));
#11453=DIRECTION('center_axis',(-1.,0.,0.));
#11454=DIRECTION('ref_axis',(0.,-1.,0.));
#11455=DIRECTION('center_axis',(-1.,0.,0.));
#11456=DIRECTION('ref_axis',(0.,-1.,0.));
#11457=DIRECTION('',(-0.707106781186547,0.707106781186548,8.65956056235494E-17));
#11458=DIRECTION('center_axis',(1.,0.,0.));
#11459=DIRECTION('ref_axis',(0.,-1.,0.));
#11460=DIRECTION('center_axis',(1.,0.,0.));
#11461=DIRECTION('ref_axis',(0.,-1.,0.));
#11462=DIRECTION('center_axis',(1.,0.,0.));
#11463=DIRECTION('ref_axis',(0.,1.,0.));
#11464=DIRECTION('',(-1.,0.,0.));
#11465=DIRECTION('center_axis',(1.,0.,0.));
#11466=DIRECTION('ref_axis',(0.,0.,-1.));
#11467=DIRECTION('center_axis',(1.,0.,0.));
#11468=DIRECTION('ref_axis',(0.,0.,-1.));
#11469=DIRECTION('center_axis',(-0.707106781186549,0.,0.707106781186546));
#11470=DIRECTION('ref_axis',(0.707106781186546,0.,0.707106781186549));
#11471=DIRECTION('',(0.,-1.,0.));
#11472=DIRECTION('',(0.,1.,0.));
#11473=DIRECTION('center_axis',(1.,0.,0.));
#11474=DIRECTION('ref_axis',(0.,-1.83697019872103E-16,-1.));
#11475=DIRECTION('center_axis',(1.,0.,0.));
#11476=DIRECTION('ref_axis',(0.,0.,-1.));
#11477=DIRECTION('center_axis',(1.,0.,0.));
#11478=DIRECTION('ref_axis',(0.,0.,-1.));
#11479=DIRECTION('center_axis',(1.,0.,0.));
#11480=DIRECTION('ref_axis',(0.,0.,-1.));
#11481=DIRECTION('center_axis',(-1.,0.,0.));
#11482=DIRECTION('ref_axis',(0.,0.,1.));
#11483=DIRECTION('center_axis',(1.,0.,0.));
#11484=DIRECTION('ref_axis',(0.,0.,-1.));
#11485=DIRECTION('center_axis',(1.,0.,0.));
#11486=DIRECTION('ref_axis',(0.,1.,0.));
#11487=DIRECTION('',(0.,1.,0.));
#11488=DIRECTION('center_axis',(0.,0.,-1.));
#11489=DIRECTION('ref_axis',(0.,1.,0.));
#11490=DIRECTION('',(-1.,0.,0.));
#11491=DIRECTION('',(1.,0.,0.));
#11492=DIRECTION('center_axis',(1.,0.,0.));
#11493=DIRECTION('ref_axis',(0.,1.,0.));
#11494=DIRECTION('center_axis',(1.,0.,0.));
#11495=DIRECTION('ref_axis',(0.,0.,-1.));
#11496=DIRECTION('',(-1.,0.,0.));
#11497=DIRECTION('center_axis',(-1.,0.,0.));
#11498=DIRECTION('ref_axis',(0.,0.,1.));
#11499=DIRECTION('center_axis',(1.,0.,0.));
#11500=DIRECTION('ref_axis',(0.,0.,-1.));
#11501=DIRECTION('center_axis',(1.,0.,0.));
#11502=DIRECTION('ref_axis',(0.,1.,0.));
#11503=DIRECTION('',(-0.707106781186547,0.707106781186548,8.65956056235494E-17));
#11504=DIRECTION('axis',(0.,0.,1.));
#11505=DIRECTION('refdir',(1.,0.,0.));
#11506=DIRECTION('center_axis',(1.,0.,0.));
#11507=DIRECTION('ref_axis',(0.,-1.,0.));
#11508=DIRECTION('center_axis',(-1.,0.,0.));
#11509=DIRECTION('ref_axis',(0.,-1.,0.));
#11510=DIRECTION('center_axis',(-1.,0.,0.));
#11511=DIRECTION('ref_axis',(0.,-1.,0.));
#11512=DIRECTION('',(-0.707106781186548,-0.707106781186547,-8.65956056235492E-17));
#11513=DIRECTION('center_axis',(1.,0.,0.));
#11514=DIRECTION('ref_axis',(0.,-1.,0.));
#11515=DIRECTION('center_axis',(-1.,0.,0.));
#11516=DIRECTION('ref_axis',(0.,0.,1.));
#11517=DIRECTION('center_axis',(1.,0.,0.));
#11518=DIRECTION('ref_axis',(0.,1.,0.));
#11519=DIRECTION('center_axis',(1.,0.,0.));
#11520=DIRECTION('ref_axis',(0.,0.,-1.));
#11521=DIRECTION('',(-1.,0.,0.));
#11522=DIRECTION('center_axis',(-1.,0.,0.));
#11523=DIRECTION('ref_axis',(0.,1.,0.));
#11524=DIRECTION('center_axis',(1.,0.,0.));
#11525=DIRECTION('ref_axis',(0.,0.,-1.));
#11526=DIRECTION('',(-0.707106781186547,-0.707106781186548,-8.65956056235494E-17));
#11527=DIRECTION('center_axis',(1.,0.,0.));
#11528=DIRECTION('ref_axis',(0.,0.,-1.));
#11529=DIRECTION('center_axis',(1.,0.,0.));
#11530=DIRECTION('ref_axis',(0.,0.,-1.));
#11531=DIRECTION('center_axis',(1.,0.,0.));
#11532=DIRECTION('ref_axis',(0.,1.,0.));
#11533=DIRECTION('center_axis',(1.,0.,0.));
#11534=DIRECTION('ref_axis',(0.,0.,-1.));
#11535=DIRECTION('',(-1.,0.,0.));
#11536=DIRECTION('center_axis',(-1.,0.,0.));
#11537=DIRECTION('ref_axis',(0.,1.,0.));
#11538=DIRECTION('center_axis',(1.,0.,0.));
#11539=DIRECTION('ref_axis',(0.,0.,-1.));
#11540=DIRECTION('',(-0.707106781186547,-0.707106781186548,-8.65956056235494E-17));
#11541=DIRECTION('center_axis',(1.,0.,0.));
#11542=DIRECTION('ref_axis',(0.,0.,-1.));
#11543=DIRECTION('axis',(0.,0.,1.));
#11544=DIRECTION('refdir',(1.,0.,0.));
#11545=DIRECTION('center_axis',(1.,0.,0.));
#11546=DIRECTION('ref_axis',(0.,-1.,0.));
#11547=DIRECTION('center_axis',(-1.,0.,0.));
#11548=DIRECTION('ref_axis',(0.,-1.,0.));
#11549=DIRECTION('center_axis',(-1.,0.,0.));
#11550=DIRECTION('ref_axis',(0.,-1.,0.));
#11551=DIRECTION('',(-0.707106781186547,-0.707106781186548,-8.65956056235494E-17));
#11552=DIRECTION('center_axis',(1.,0.,0.));
#11553=DIRECTION('ref_axis',(0.,-1.,0.));
#11554=DIRECTION('center_axis',(-1.,0.,0.));
#11555=DIRECTION('ref_axis',(0.,0.,1.));
#11556=DIRECTION('center_axis',(1.,0.,0.));
#11557=DIRECTION('ref_axis',(0.,0.,-1.));
#11558=DIRECTION('center_axis',(1.,0.,0.));
#11559=DIRECTION('ref_axis',(0.,1.,0.));
#11560=DIRECTION('center_axis',(1.,0.,0.));
#11561=DIRECTION('ref_axis',(0.,0.,-1.));
#11562=DIRECTION('',(-1.,0.,0.));
#11563=DIRECTION('center_axis',(1.,0.,0.));
#11564=DIRECTION('ref_axis',(0.,1.,0.));
#11565=DIRECTION('center_axis',(1.,0.,0.));
#11566=DIRECTION('ref_axis',(0.,0.,-1.));
#11567=DIRECTION('',(-1.,0.,0.));
#11568=DIRECTION('center_axis',(1.,0.,0.));
#11569=DIRECTION('ref_axis',(0.,0.,-1.));
#11570=DIRECTION('center_axis',(1.,0.,0.));
#11571=DIRECTION('ref_axis',(0.,0.,-1.));
#11572=DIRECTION('center_axis',(1.,0.,0.));
#11573=DIRECTION('ref_axis',(0.,1.,0.));
#11574=DIRECTION('center_axis',(1.,0.,0.));
#11575=DIRECTION('ref_axis',(0.,0.,-1.));
#11576=DIRECTION('',(-1.,0.,0.));
#11577=DIRECTION('center_axis',(1.,0.,0.));
#11578=DIRECTION('ref_axis',(0.,0.,-1.));
#11579=DIRECTION('axis',(0.,0.,1.));
#11580=DIRECTION('refdir',(1.,0.,0.));
#11581=DIRECTION('center_axis',(1.,0.,0.));
#11582=DIRECTION('ref_axis',(0.,0.707106781186547,-0.707106781186548));
#11583=DIRECTION('',(0.707106781186548,0.707106781186548,0.));
#11584=DIRECTION('center_axis',(-1.,0.,0.));
#11585=DIRECTION('ref_axis',(0.,0.707106781186547,-0.707106781186548));
#11586=DIRECTION('',(0.707106781186548,0.,-0.707106781186547));
#11587=DIRECTION('center_axis',(1.,0.,0.));
#11588=DIRECTION('ref_axis',(0.,0.707106781186547,-0.707106781186548));
#11589=DIRECTION('center_axis',(-0.707106781186548,0.707106781186548,0.));
#11590=DIRECTION('ref_axis',(0.,0.,1.));
#11591=DIRECTION('',(0.,0.,1.));
#11592=DIRECTION('center_axis',(-0.707106781186548,0.707106781186548,0.));
#11593=DIRECTION('ref_axis',(0.707106781186547,0.707106781186547,0.));
#11594=DIRECTION('',(0.,0.,-1.));
#11595=DIRECTION('center_axis',(1.,0.,0.));
#11596=DIRECTION('ref_axis',(0.,0.,-1.));
#11597=DIRECTION('',(0.,1.,0.));
#11598=DIRECTION('center_axis',(1.,0.,0.));
#11599=DIRECTION('ref_axis',(0.,-0.707106781186547,-0.707106781186548));
#11600=DIRECTION('',(0.,0.,-1.));
#11601=DIRECTION('center_axis',(1.,0.,0.));
#11602=DIRECTION('ref_axis',(0.,0.,-1.));
#11603=DIRECTION('center_axis',(1.,0.,0.));
#11604=DIRECTION('ref_axis',(0.,-0.707106781186547,-0.707106781186548));
#11605=DIRECTION('',(0.707106781186548,0.,-0.707106781186547));
#11606=DIRECTION('center_axis',(-1.,0.,0.));
#11607=DIRECTION('ref_axis',(0.,-0.707106781186547,-0.707106781186548));
#11608=DIRECTION('',(0.707106781186548,-0.707106781186548,0.));
#11609=DIRECTION('center_axis',(-0.707106781186548,0.,-0.707106781186548));
#11610=DIRECTION('ref_axis',(-0.707106781186548,0.,0.707106781186548));
#11611=DIRECTION('',(0.,-1.,0.));
#11612=DIRECTION('center_axis',(1.,0.,0.));
#11613=DIRECTION('ref_axis',(0.,0.707106781186547,0.707106781186548));
#11614=DIRECTION('',(0.707106781186548,0.,0.707106781186547));
#11615=DIRECTION('center_axis',(-1.,0.,0.));
#11616=DIRECTION('ref_axis',(0.,0.707106781186547,0.707106781186548));
#11617=DIRECTION('',(0.707106781186548,0.707106781186548,0.));
#11618=DIRECTION('center_axis',(1.,0.,0.));
#11619=DIRECTION('ref_axis',(0.,0.707106781186547,0.707106781186548));
#11620=DIRECTION('center_axis',(-0.707106781186548,0.,0.707106781186548));
#11621=DIRECTION('ref_axis',(0.707106781186548,0.,0.707106781186548));
#11622=DIRECTION('',(0.,-1.,0.));
#11623=DIRECTION('',(0.707106781186548,0.,0.707106781186547));
#11624=DIRECTION('',(0.,1.,0.));
#11625=DIRECTION('center_axis',(1.,0.,0.));
#11626=DIRECTION('ref_axis',(0.,0.,-1.));
#11627=DIRECTION('',(0.,0.,1.));
#11628=DIRECTION('center_axis',(1.,0.,0.));
#11629=DIRECTION('ref_axis',(0.,0.,-1.));
#11630=DIRECTION('',(0.,0.,-1.));
#11631=DIRECTION('center_axis',(1.,0.,0.));
#11632=DIRECTION('ref_axis',(0.,-0.707106781186547,0.707106781186548));
#11633=DIRECTION('center_axis',(1.,0.,0.));
#11634=DIRECTION('ref_axis',(0.,-0.707106781186547,0.707106781186548));
#11635=DIRECTION('',(0.707106781186548,-0.707106781186548,0.));
#11636=DIRECTION('center_axis',(-1.,0.,0.));
#11637=DIRECTION('ref_axis',(0.,-0.707106781186547,0.707106781186548));
#11638=DIRECTION('center_axis',(-0.707106781186548,-0.707106781186548,0.));
#11639=DIRECTION('ref_axis',(0.,0.,1.));
#11640=DIRECTION('center_axis',(-0.707106781186548,-0.707106781186548,0.));
#11641=DIRECTION('ref_axis',(-0.707106781186547,0.707106781186547,0.));
#11642=DIRECTION('',(0.,0.,1.));
#11643=DIRECTION('',(0.707106781186547,-6.86915450674151E-16,-0.707106781186548));
#11644=DIRECTION('center_axis',(0.,0.,-1.));
#11645=DIRECTION('ref_axis',(1.,0.,0.));
#11646=DIRECTION('',(0.,0.,-1.));
#11647=DIRECTION('center_axis',(1.,0.,0.));
#11648=DIRECTION('ref_axis',(0.,1.,0.));
#11649=DIRECTION('center_axis',(0.707106781186548,0.707106781186548,0.));
#11650=DIRECTION('ref_axis',(-0.707106781186547,0.707106781186547,0.));
#11651=DIRECTION('center_axis',(-0.707106781186548,-0.707106781186548,0.));
#11652=DIRECTION('ref_axis',(-0.707106781186547,0.707106781186547,0.));
#11653=DIRECTION('center_axis',(0.707106781186548,-0.707106781186548,0.));
#11654=DIRECTION('ref_axis',(0.707106781186547,0.707106781186547,0.));
#11655=DIRECTION('center_axis',(1.,0.,0.));
#11656=DIRECTION('ref_axis',(0.,0.,-1.));
#11657=DIRECTION('',(-1.,0.,0.));
#11658=DIRECTION('center_axis',(1.,0.,0.));
#11659=DIRECTION('ref_axis',(0.,0.,-1.));
#11660=DIRECTION('center_axis',(1.,0.,0.));
#11661=DIRECTION('ref_axis',(0.,0.,-1.));
#11662=DIRECTION('center_axis',(0.707106781186548,-0.707106781186548,0.));
#11663=DIRECTION('ref_axis',(0.707106781186547,0.707106781186547,0.));
#11664=DIRECTION('center_axis',(-0.707106781186548,0.707106781186548,0.));
#11665=DIRECTION('ref_axis',(0.707106781186547,0.707106781186547,0.));
#11666=DIRECTION('center_axis',(0.707106781186548,0.707106781186548,0.));
#11667=DIRECTION('ref_axis',(-0.707106781186547,0.707106781186547,0.));
#11668=DIRECTION('center_axis',(1.,0.,0.));
#11669=DIRECTION('ref_axis',(0.,0.,-1.));
#11670=DIRECTION('center_axis',(1.,0.,0.));
#11671=DIRECTION('ref_axis',(0.,0.,-1.));
#11672=DIRECTION('center_axis',(1.,0.,0.));
#11673=DIRECTION('ref_axis',(0.,0.,-1.));
#11674=DIRECTION('center_axis',(-0.707106781186546,0.707106781186549,0.));
#11675=DIRECTION('ref_axis',(-0.707106781186549,-0.707106781186546,0.));
#11676=DIRECTION('',(0.,0.,1.));
#11677=DIRECTION('',(0.,0.,-1.));
#11678=DIRECTION('center_axis',(-0.707106781186545,-0.70710678118655,0.));
#11679=DIRECTION('ref_axis',(0.70710678118655,-0.707106781186545,0.));
#11680=DIRECTION('',(0.,0.,1.));
#11681=DIRECTION('center_axis',(-0.707106781186546,0.707106781186549,0.));
#11682=DIRECTION('ref_axis',(-0.707106781186549,-0.707106781186546,0.));
#11683=DIRECTION('',(0.577350269189626,0.577350269189625,-0.577350269189626));
#11684=DIRECTION('',(0.,0.,1.));
#11685=DIRECTION('',(-0.577350269189626,-0.577350269189625,-0.577350269189626));
#11686=DIRECTION('',(0.,0.,-1.));
#11687=DIRECTION('center_axis',(-0.707106781186546,-0.707106781186549,0.));
#11688=DIRECTION('ref_axis',(0.707106781186549,-0.707106781186546,0.));
#11689=DIRECTION('',(-0.577350269189626,0.577350269189625,0.577350269189626));
#11690=DIRECTION('',(0.,0.,1.));
#11691=DIRECTION('',(0.577350269189626,-0.577350269189625,0.577350269189626));
#11692=DIRECTION('center_axis',(-0.707106781186546,0.707106781186549,0.));
#11693=DIRECTION('ref_axis',(-0.707106781186549,-0.707106781186546,0.));
#11694=DIRECTION('',(0.577350269189627,0.577350269189624,-0.577350269189627));
#11695=DIRECTION('',(0.,0.,1.));
#11696=DIRECTION('',(-0.577350269189627,-0.577350269189624,-0.577350269189627));
#11697=DIRECTION('',(0.,0.,-1.));
#11698=DIRECTION('center_axis',(-0.707106781186546,-0.707106781186549,0.));
#11699=DIRECTION('ref_axis',(0.707106781186549,-0.707106781186546,0.));
#11700=DIRECTION('',(-0.577350269189627,0.577350269189624,0.577350269189627));
#11701=DIRECTION('',(0.,0.,1.));
#11702=DIRECTION('',(0.577350269189626,-0.577350269189624,0.577350269189626));
#11703=DIRECTION('center_axis',(-0.707106781186546,0.707106781186549,0.));
#11704=DIRECTION('ref_axis',(-0.707106781186549,-0.707106781186546,0.));
#11705=DIRECTION('',(0.577350269189627,0.577350269189624,-0.577350269189627));
#11706=DIRECTION('',(0.,0.,1.));
#11707=DIRECTION('',(-0.577350269189627,-0.577350269189624,-0.577350269189627));
#11708=DIRECTION('',(0.,0.,-1.));
#11709=DIRECTION('center_axis',(-0.707106781186546,-0.707106781186549,0.));
#11710=DIRECTION('ref_axis',(0.707106781186549,-0.707106781186546,0.));
#11711=DIRECTION('',(-0.577350269189627,0.577350269189624,0.577350269189627));
#11712=DIRECTION('',(0.,0.,1.));
#11713=DIRECTION('',(0.577350269189627,-0.577350269189624,0.577350269189627));
#11714=DIRECTION('center_axis',(-0.707106781186546,0.707106781186549,0.));
#11715=DIRECTION('ref_axis',(-0.707106781186549,-0.707106781186546,0.));
#11716=DIRECTION('',(0.577350269189626,0.577350269189625,-0.577350269189626));
#11717=DIRECTION('',(0.,0.,1.));
#11718=DIRECTION('',(-0.577350269189626,-0.577350269189625,-0.577350269189626));
#11719=DIRECTION('',(0.,0.,-1.));
#11720=DIRECTION('center_axis',(-0.707106781186546,-0.707106781186549,0.));
#11721=DIRECTION('ref_axis',(0.707106781186549,-0.707106781186546,0.));
#11722=DIRECTION('',(-0.577350269189627,0.577350269189624,0.577350269189627));
#11723=DIRECTION('',(0.,0.,1.));
#11724=DIRECTION('',(0.577350269189627,-0.577350269189624,0.577350269189627));
#11725=DIRECTION('center_axis',(-0.707106781186545,-0.70710678118655,0.));
#11726=DIRECTION('ref_axis',(0.70710678118655,-0.707106781186545,0.));
#11727=DIRECTION('',(0.,0.,1.));
#11728=DIRECTION('',(0.,0.,1.));
#11729=DIRECTION('center_axis',(-0.707106781186546,0.707106781186549,0.));
#11730=DIRECTION('ref_axis',(-0.707106781186549,-0.707106781186546,0.));
#11731=DIRECTION('',(0.,0.,-1.));
#11732=DIRECTION('center_axis',(-0.707106781186546,-0.707106781186549,0.));
#11733=DIRECTION('ref_axis',(0.707106781186549,-0.707106781186546,0.));
#11734=DIRECTION('',(0.,0.,1.));
#11735=DIRECTION('',(0.,0.,1.));
#11736=DIRECTION('center_axis',(-0.707106781186545,0.70710678118655,0.));
#11737=DIRECTION('ref_axis',(-0.70710678118655,-0.707106781186545,0.));
#11738=DIRECTION('',(0.,0.,-1.));
#11739=DIRECTION('center_axis',(-0.707106781186546,0.707106781186549,0.));
#11740=DIRECTION('ref_axis',(-0.707106781186549,-0.707106781186546,0.));
#11741=DIRECTION('',(0.577350269189627,0.577350269189624,-0.577350269189627));
#11742=DIRECTION('',(0.,0.,1.));
#11743=DIRECTION('',(-0.577350269189627,-0.577350269189624,-0.577350269189627));
#11744=DIRECTION('',(0.,0.,-1.));
#11745=DIRECTION('center_axis',(-0.707106781186546,-0.707106781186549,0.));
#11746=DIRECTION('ref_axis',(0.707106781186549,-0.707106781186546,0.));
#11747=DIRECTION('',(-0.577350269189626,0.577350269189625,0.577350269189626));
#11748=DIRECTION('',(0.,0.,1.));
#11749=DIRECTION('',(0.577350269189626,-0.577350269189625,0.577350269189626));
#11750=DIRECTION('center_axis',(-0.707106781186546,0.707106781186549,0.));
#11751=DIRECTION('ref_axis',(-0.707106781186549,-0.707106781186546,0.));
#11752=DIRECTION('',(0.577350269189627,0.577350269189624,-0.577350269189627));
#11753=DIRECTION('',(0.,0.,1.));
#11754=DIRECTION('',(-0.577350269189626,-0.577350269189624,-0.577350269189626));
#11755=DIRECTION('',(0.,0.,-1.));
#11756=DIRECTION('center_axis',(-0.707106781186546,-0.707106781186549,0.));
#11757=DIRECTION('ref_axis',(0.707106781186549,-0.707106781186546,0.));
#11758=DIRECTION('',(-0.577350269189627,0.577350269189624,0.577350269189627));
#11759=DIRECTION('',(0.,0.,1.));
#11760=DIRECTION('',(0.577350269189626,-0.577350269189624,0.577350269189626));
#11761=DIRECTION('center_axis',(-0.707106781186546,-0.707106781186549,0.));
#11762=DIRECTION('ref_axis',(0.707106781186549,-0.707106781186546,0.));
#11763=DIRECTION('',(0.,0.,1.));
#11764=DIRECTION('',(0.,0.,1.));
#11765=DIRECTION('center_axis',(-0.707106781186545,0.70710678118655,0.));
#11766=DIRECTION('ref_axis',(-0.70710678118655,-0.707106781186545,0.));
#11767=DIRECTION('',(0.,0.,-1.));
#11768=DIRECTION('center_axis',(-0.707106781186546,0.707106781186549,0.));
#11769=DIRECTION('ref_axis',(-0.707106781186549,-0.707106781186546,0.));
#11770=DIRECTION('',(0.577350269189626,0.577350269189625,-0.577350269189626));
#11771=DIRECTION('',(0.,0.,1.));
#11772=DIRECTION('',(-0.577350269189626,-0.577350269189625,-0.577350269189626));
#11773=DIRECTION('',(0.,0.,-1.));
#11774=DIRECTION('center_axis',(-0.707106781186546,-0.707106781186549,0.));
#11775=DIRECTION('ref_axis',(0.707106781186549,-0.707106781186546,0.));
#11776=DIRECTION('',(-0.577350269189627,0.577350269189624,0.577350269189627));
#11777=DIRECTION('',(0.,0.,1.));
#11778=DIRECTION('',(0.577350269189627,-0.577350269189624,0.577350269189627));
#11779=DIRECTION('center_axis',(-0.707106781186545,0.70710678118655,0.));
#11780=DIRECTION('ref_axis',(-0.70710678118655,-0.707106781186545,0.));
#11781=DIRECTION('',(0.,0.,1.));
#11782=DIRECTION('',(0.,0.,-1.));
#11783=DIRECTION('center_axis',(-0.707106781186546,-0.707106781186549,0.));
#11784=DIRECTION('ref_axis',(0.707106781186549,-0.707106781186546,0.));
#11785=DIRECTION('',(0.,0.,1.));
#11786=DIRECTION('center_axis',(-0.707106781186546,-0.707106781186549,0.));
#11787=DIRECTION('ref_axis',(0.707106781186549,-0.707106781186546,0.));
#11788=DIRECTION('',(0.,0.,1.));
#11789=DIRECTION('',(0.,0.,1.));
#11790=DIRECTION('center_axis',(-0.707106781186545,0.70710678118655,0.));
#11791=DIRECTION('ref_axis',(-0.70710678118655,-0.707106781186545,0.));
#11792=DIRECTION('',(0.,0.,-1.));
#11793=DIRECTION('center_axis',(-1.,0.,0.));
#11794=DIRECTION('ref_axis',(0.,-0.707106781186547,0.707106781186548));
#11795=DIRECTION('center_axis',(-1.,0.,0.));
#11796=DIRECTION('ref_axis',(0.,-0.707106781186547,0.707106781186548));
#11797=DIRECTION('',(-0.707106781186547,-7.85046229341887E-16,0.707106781186547));
#11798=DIRECTION('center_axis',(1.,0.,0.));
#11799=DIRECTION('ref_axis',(0.,-0.707106781186547,0.707106781186548));
#11800=DIRECTION('',(-0.707106781186547,-0.707106781186547,0.));
#11801=DIRECTION('center_axis',(-1.,0.,0.));
#11802=DIRECTION('ref_axis',(0.,-0.707106781186547,0.707106781186548));
#11803=DIRECTION('center_axis',(-1.,0.,0.));
#11804=DIRECTION('ref_axis',(0.,-0.707106781186547,0.707106781186548));
#11805=DIRECTION('center_axis',(0.707106781186548,0.,0.707106781186548));
#11806=DIRECTION('ref_axis',(0.707106781186548,0.,-0.707106781186548));
#11807=DIRECTION('',(0.,1.,0.));
#11808=DIRECTION('',(-0.707106781186547,0.,0.707106781186547));
#11809=DIRECTION('',(0.,-1.,0.));
#11810=DIRECTION('',(0.,1.,0.));
#11811=DIRECTION('',(0.,1.,0.));
#11812=DIRECTION('',(0.,1.,0.));
#11813=DIRECTION('',(0.,1.,0.));
#11814=DIRECTION('',(0.,1.,0.));
#11815=DIRECTION('',(0.,1.,0.));
#11816=DIRECTION('',(0.,1.,0.));
#11817=DIRECTION('center_axis',(1.,0.,0.));
#11818=DIRECTION('ref_axis',(0.,0.,-1.));
#11819=DIRECTION('center_axis',(-1.,0.,0.));
#11820=DIRECTION('ref_axis',(0.,0.707106781186547,-0.707106781186548));
#11821=DIRECTION('center_axis',(-1.,0.,0.));
#11822=DIRECTION('ref_axis',(0.,0.707106781186547,0.707106781186548));
#11823=DIRECTION('center_axis',(1.,0.,0.));
#11824=DIRECTION('ref_axis',(0.,0.,-1.));
#11825=DIRECTION('',(0.,-1.,0.));
#11826=DIRECTION('center_axis',(-1.,0.,0.));
#11827=DIRECTION('ref_axis',(0.,0.707106781186547,-0.707106781186548));
#11828=DIRECTION('center_axis',(-1.,0.,0.));
#11829=DIRECTION('ref_axis',(0.,0.707106781186547,0.707106781186548));
#11830=DIRECTION('center_axis',(1.,0.,0.));
#11831=DIRECTION('ref_axis',(0.,0.,-1.));
#11832=DIRECTION('',(0.,-1.,0.));
#11833=DIRECTION('center_axis',(1.,0.,0.));
#11834=DIRECTION('ref_axis',(0.,0.,-1.));
#11835=DIRECTION('',(0.,-1.,0.));
#11836=DIRECTION('center_axis',(1.,0.,0.));
#11837=DIRECTION('ref_axis',(0.,0.,-1.));
#11838=DIRECTION('center_axis',(-1.,0.,0.));
#11839=DIRECTION('ref_axis',(0.,-0.707106781186547,-0.707106781186548));
#11840=DIRECTION('center_axis',(1.,0.,0.));
#11841=DIRECTION('ref_axis',(0.,0.,-1.));
#11842=DIRECTION('center_axis',(-1.,0.,0.));
#11843=DIRECTION('ref_axis',(0.,-0.707106781186547,-0.707106781186548));
#11844=DIRECTION('center_axis',(1.,0.,0.));
#11845=DIRECTION('ref_axis',(0.,0.,-1.));
#11846=DIRECTION('center_axis',(-1.,0.,0.));
#11847=DIRECTION('ref_axis',(0.,-0.707106781186547,-0.707106781186548));
#11848=DIRECTION('',(0.,-1.,0.));
#11849=DIRECTION('center_axis',(1.,0.,0.));
#11850=DIRECTION('ref_axis',(0.,0.,-1.));
#11851=DIRECTION('',(0.,-1.,0.));
#11852=DIRECTION('center_axis',(1.,0.,0.));
#11853=DIRECTION('ref_axis',(0.,0.,-1.));
#11854=DIRECTION('',(0.,-1.,0.));
#11855=DIRECTION('center_axis',(1.,0.,0.));
#11856=DIRECTION('ref_axis',(0.,0.,-1.));
#11857=DIRECTION('',(0.,-1.,0.));
#11858=DIRECTION('center_axis',(1.,0.,0.));
#11859=DIRECTION('ref_axis',(0.,0.,-1.));
#11860=DIRECTION('',(0.,-1.,0.));
#11861=DIRECTION('center_axis',(-1.,0.,0.));
#11862=DIRECTION('ref_axis',(0.,0.707106781186547,0.707106781186548));
#11863=DIRECTION('',(-0.707106781186549,0.707106781186546,0.));
#11864=DIRECTION('center_axis',(1.,0.,0.));
#11865=DIRECTION('ref_axis',(0.,0.707106781186547,0.707106781186548));
#11866=DIRECTION('center_axis',(-1.,0.,0.));
#11867=DIRECTION('ref_axis',(0.,0.707106781186547,0.707106781186548));
#11868=DIRECTION('center_axis',(0.707106781186548,-0.707106781186548,0.));
#11869=DIRECTION('ref_axis',(0.,0.,-1.));
#11870=DIRECTION('',(0.,0.,1.));
#11871=DIRECTION('',(0.,0.,-1.));
#11872=DIRECTION('center_axis',(0.,-1.,0.));
#11873=DIRECTION('ref_axis',(0.,0.,-1.));
#11874=DIRECTION('',(0.,0.,1.));
#11875=DIRECTION('',(-1.,0.,0.));
#11876=DIRECTION('',(0.,0.,-1.));
#11877=DIRECTION('',(1.,0.,0.));
#11878=DIRECTION('center_axis',(0.707106781186548,0.707106781186548,0.));
#11879=DIRECTION('ref_axis',(0.,0.,-1.));
#11880=DIRECTION('',(0.,0.,-1.));
#11881=DIRECTION('',(0.,0.,1.));
#11882=DIRECTION('center_axis',(0.,1.,0.));
#11883=DIRECTION('ref_axis',(0.,0.,1.));
#11884=DIRECTION('',(0.,0.,-1.));
#11885=DIRECTION('',(-1.,0.,0.));
#11886=DIRECTION('',(0.,0.,1.));
#11887=DIRECTION('',(1.,0.,0.));
#11888=DIRECTION('center_axis',(1.,0.,0.));
#11889=DIRECTION('ref_axis',(0.,-0.707106781186547,0.707106781186548));
#11890=DIRECTION('',(-1.,0.,0.));
#11891=DIRECTION('center_axis',(-0.707106781186548,-0.707106781186548,0.));
#11892=DIRECTION('ref_axis',(0.,0.,1.));
#11893=DIRECTION('center_axis',(1.,0.,0.));
#11894=DIRECTION('ref_axis',(0.,-0.707106781186547,-0.707106781186548));
#11895=DIRECTION('',(1.,0.,0.));
#11896=DIRECTION('center_axis',(1.,0.,0.));
#11897=DIRECTION('ref_axis',(0.,-0.707106781186547,-0.707106781186548));
#11898=DIRECTION('center_axis',(-0.707106781186548,0.707106781186548,0.));
#11899=DIRECTION('ref_axis',(0.,0.,1.));
#11900=DIRECTION('center_axis',(1.,0.,0.));
#11901=DIRECTION('ref_axis',(0.,0.707106781186547,-0.707106781186548));
#11902=DIRECTION('center_axis',(1.,0.,0.));
#11903=DIRECTION('ref_axis',(0.,0.707106781186547,-0.707106781186548));
#11904=DIRECTION('',(-1.,0.,0.));
#11905=DIRECTION('center_axis',(0.,0.,-1.));
#11906=DIRECTION('ref_axis',(0.,1.,0.));
#11907=DIRECTION('',(0.,1.,0.));
#11908=DIRECTION('center_axis',(-1.,0.,0.));
#11909=DIRECTION('ref_axis',(0.,-0.707106781186547,-0.707106781186548));
#11910=DIRECTION('',(-0.707106781186549,-0.707106781186546,0.));
#11911=DIRECTION('',(0.707106781186547,-7.85046229341887E-16,0.707106781186547));
#11912=DIRECTION('center_axis',(0.707106781186548,-0.707106781186548,0.));
#11913=DIRECTION('ref_axis',(0.,0.,-1.));
#11914=DIRECTION('center_axis',(0.707106781186548,0.707106781186548,0.));
#11915=DIRECTION('ref_axis',(0.,0.,-1.));
#11916=DIRECTION('',(-0.707106781186547,0.707106781186547,0.));
#11917=DIRECTION('center_axis',(-1.,0.,0.));
#11918=DIRECTION('ref_axis',(0.,0.707106781186547,-0.707106781186548));
#11919=DIRECTION('center_axis',(-1.,0.,0.));
#11920=DIRECTION('ref_axis',(0.,0.707106781186547,-0.707106781186548));
#11921=DIRECTION('',(-0.707106781186547,7.85046229341887E-16,-0.707106781186547));
#11922=DIRECTION('center_axis',(0.707106781186548,0.,-0.707106781186548));
#11923=DIRECTION('ref_axis',(-0.707106781186548,0.,-0.707106781186548));
#11924=DIRECTION('center_axis',(1.,0.,0.));
#11925=DIRECTION('ref_axis',(0.,0.,-1.));
#11926=DIRECTION('center_axis',(1.,0.,0.));
#11927=DIRECTION('ref_axis',(0.,0.707106781186547,0.707106781186548));
#11928=DIRECTION('',(1.,0.,0.));
#11929=DIRECTION('center_axis',(0.,0.,1.));
#11930=DIRECTION('ref_axis',(0.,-1.,0.));
#11931=DIRECTION('center_axis',(1.,0.,0.));
#11932=DIRECTION('ref_axis',(0.,0.,-1.));
#11933=DIRECTION('center_axis',(1.,0.,0.));
#11934=DIRECTION('ref_axis',(0.,0.,-1.));
#11935=DIRECTION('center_axis',(1.,0.,0.));
#11936=DIRECTION('ref_axis',(0.,1.,0.));
#11937=DIRECTION('',(-1.,0.,0.));
#11938=DIRECTION('center_axis',(1.,0.,0.));
#11939=DIRECTION('ref_axis',(0.,0.,-1.));
#11940=DIRECTION('center_axis',(-1.,0.,0.));
#11941=DIRECTION('ref_axis',(0.,0.,1.));
#11942=DIRECTION('center_axis',(1.,0.,0.));
#11943=DIRECTION('ref_axis',(0.,0.,-1.));
#11944=DIRECTION('center_axis',(1.,0.,0.));
#11945=DIRECTION('ref_axis',(0.,1.,0.));
#11946=DIRECTION('',(-0.707106781186547,0.707106781186548,8.65956056235494E-17));
#11947=DIRECTION('axis',(0.,0.,1.));
#11948=DIRECTION('refdir',(1.,0.,0.));
#11949=DIRECTION('center_axis',(1.,0.,0.));
#11950=DIRECTION('ref_axis',(0.,1.,0.));
#11951=DIRECTION('',(-1.,0.,0.));
#11952=DIRECTION('center_axis',(1.,0.,0.));
#11953=DIRECTION('ref_axis',(0.,1.,0.));
#11954=DIRECTION('center_axis',(1.,0.,0.));
#11955=DIRECTION('ref_axis',(0.,1.,0.));
#11956=DIRECTION('',(-1.,0.,0.));
#11957=DIRECTION('center_axis',(1.,0.,0.));
#11958=DIRECTION('ref_axis',(0.,1.,0.));
#11959=DIRECTION('',(-1.,0.,0.));
#11960=DIRECTION('center_axis',(1.,0.,0.));
#11961=DIRECTION('ref_axis',(0.,1.,0.));
#11962=DIRECTION('',(-1.,0.,0.));
#11963=DIRECTION('center_axis',(1.,0.,0.));
#11964=DIRECTION('ref_axis',(0.,1.,0.));
#11965=DIRECTION('',(-1.,0.,0.));
#11966=DIRECTION('center_axis',(1.,0.,0.));
#11967=DIRECTION('ref_axis',(0.,1.,4.77055255383026E-15));
#11968=DIRECTION('',(1.,0.,0.));
#11969=DIRECTION('center_axis',(1.,0.,0.));
#11970=DIRECTION('ref_axis',(0.,1.,4.77055255383026E-15));
#11971=DIRECTION('center_axis',(1.,0.,0.));
#11972=DIRECTION('ref_axis',(0.,1.,4.77055255383026E-15));
#11973=DIRECTION('',(1.,0.,0.));
#11974=DIRECTION('center_axis',(1.,0.,0.));
#11975=DIRECTION('ref_axis',(0.,1.,4.77055255383026E-15));
#11976=DIRECTION('center_axis',(1.,0.,0.));
#11977=DIRECTION('ref_axis',(0.,1.,4.77055255383026E-15));
#11978=DIRECTION('',(1.,0.,0.));
#11979=DIRECTION('center_axis',(1.,0.,0.));
#11980=DIRECTION('ref_axis',(0.,1.,4.77055255383026E-15));
#11981=DIRECTION('',(1.,0.,0.));
#11982=DIRECTION('center_axis',(1.,0.,0.));
#11983=DIRECTION('ref_axis',(0.,1.,4.77055255383026E-15));
#11984=DIRECTION('',(1.,0.,0.));
#11985=DIRECTION('center_axis',(1.,0.,0.));
#11986=DIRECTION('ref_axis',(0.,0.,-1.));
#11987=DIRECTION('center_axis',(-1.,0.,0.));
#11988=DIRECTION('ref_axis',(0.,1.,0.));
#11989=DIRECTION('center_axis',(-1.,0.,0.));
#11990=DIRECTION('ref_axis',(0.,1.,0.));
#11991=DIRECTION('center_axis',(1.,0.,0.));
#11992=DIRECTION('ref_axis',(0.,0.,-1.));
#11993=DIRECTION('center_axis',(1.,0.,0.));
#11994=DIRECTION('ref_axis',(0.,1.,0.));
#11995=DIRECTION('center_axis',(1.,0.,0.));
#11996=DIRECTION('ref_axis',(0.,1.,0.));
#11997=DIRECTION('center_axis',(-1.,0.,0.));
#11998=DIRECTION('ref_axis',(0.,1.,4.77055255383026E-15));
#11999=DIRECTION('center_axis',(1.,0.,0.));
#12000=DIRECTION('ref_axis',(0.,1.,4.77055255383026E-15));
#12001=DIRECTION('center_axis',(0.,0.5,0.866025403784439));
#12002=DIRECTION('ref_axis',(0.,0.866025403784439,-0.5));
#12003=DIRECTION('',(0.,0.866025403784439,-0.5));
#12004=DIRECTION('',(-1.,0.,0.));
#12005=DIRECTION('',(0.,0.866025403784439,-0.5));
#12006=DIRECTION('',(-1.,0.,0.));
#12007=DIRECTION('center_axis',(0.,-0.5,0.866025403784439));
#12008=DIRECTION('ref_axis',(0.,0.866025403784439,0.5));
#12009=DIRECTION('',(0.,0.866025403784439,0.5));
#12010=DIRECTION('',(-1.,0.,0.));
#12011=DIRECTION('',(0.,0.866025403784439,0.5));
#12012=DIRECTION('center_axis',(0.,-1.,-1.20185167898973E-16));
#12013=DIRECTION('ref_axis',(0.,-1.20185167898973E-16,1.));
#12014=DIRECTION('',(0.,-1.20185167898973E-16,1.));
#12015=DIRECTION('',(-1.,0.,0.));
#12016=DIRECTION('',(0.,-1.20185167898973E-16,1.));
#12017=DIRECTION('center_axis',(0.,-0.5,-0.866025403784439));
#12018=DIRECTION('ref_axis',(0.,-0.866025403784439,0.5));
#12019=DIRECTION('',(0.,-0.866025403784439,0.5));
#12020=DIRECTION('',(-1.,0.,0.));
#12021=DIRECTION('',(0.,-0.866025403784439,0.5));
#12022=DIRECTION('center_axis',(0.,0.5,-0.866025403784439));
#12023=DIRECTION('ref_axis',(0.,-0.866025403784439,-0.5));
#12024=DIRECTION('',(0.,-0.866025403784439,-0.5));
#12025=DIRECTION('',(-1.,0.,0.));
#12026=DIRECTION('',(0.,-0.866025403784439,-0.5));
#12027=DIRECTION('center_axis',(0.,1.,-3.60555503696918E-16));
#12028=DIRECTION('ref_axis',(0.,-3.60555503696918E-16,-1.));
#12029=DIRECTION('',(0.,-3.60555503696918E-16,-1.));
#12030=DIRECTION('',(0.,-3.60555503696918E-16,-1.));
#12031=DIRECTION('center_axis',(-1.,0.,0.));
#12032=DIRECTION('ref_axis',(0.,0.,1.));
#12033=DIRECTION('center_axis',(-1.,0.,0.));
#12034=DIRECTION('ref_axis',(0.,0.,1.));
#12035=DIRECTION('center_axis',(1.,0.,0.));
#12036=DIRECTION('ref_axis',(0.,0.,-1.));
#12037=DIRECTION('center_axis',(1.,0.,0.));
#12038=DIRECTION('ref_axis',(0.,1.,0.));
#12039=DIRECTION('',(-0.707106781186547,0.707106781186548,8.65956056235494E-17));
#12040=DIRECTION('center_axis',(1.,0.,0.));
#12041=DIRECTION('ref_axis',(0.,1.,0.));
#12042=DIRECTION('center_axis',(-1.,0.,0.));
#12043=DIRECTION('ref_axis',(0.,1.,0.));
#12044=DIRECTION('center_axis',(-1.,0.,0.));
#12045=DIRECTION('ref_axis',(0.,1.,0.));
#12046=DIRECTION('center_axis',(1.,0.,0.));
#12047=DIRECTION('ref_axis',(0.,0.,-1.));
#12048=DIRECTION('',(-0.707106781186548,-0.707106781186548,-8.65956056235493E-17));
#12049=DIRECTION('center_axis',(1.,0.,0.));
#12050=DIRECTION('ref_axis',(0.,0.,-1.));
#12051=DIRECTION('axis',(0.,0.,1.));
#12052=DIRECTION('refdir',(1.,0.,0.));
#12053=DIRECTION('center_axis',(1.,0.,0.));
#12054=DIRECTION('ref_axis',(0.,1.,0.));
#12055=DIRECTION('',(-1.,0.,0.));
#12056=DIRECTION('center_axis',(1.,0.,0.));
#12057=DIRECTION('ref_axis',(0.,1.,0.));
#12058=DIRECTION('center_axis',(1.,0.,0.));
#12059=DIRECTION('ref_axis',(0.,1.,0.));
#12060=DIRECTION('',(-1.,0.,0.));
#12061=DIRECTION('center_axis',(1.,0.,0.));
#12062=DIRECTION('ref_axis',(0.,1.,0.));
#12063=DIRECTION('',(-1.,0.,0.));
#12064=DIRECTION('center_axis',(1.,0.,0.));
#12065=DIRECTION('ref_axis',(0.,1.,0.));
#12066=DIRECTION('',(-1.,0.,0.));
#12067=DIRECTION('center_axis',(1.,0.,0.));
#12068=DIRECTION('ref_axis',(0.,1.,0.));
#12069=DIRECTION('',(-1.,0.,0.));
#12070=DIRECTION('center_axis',(1.,0.,0.));
#12071=DIRECTION('ref_axis',(0.,1.,0.));
#12072=DIRECTION('',(-1.,0.,0.));
#12073=DIRECTION('center_axis',(1.,0.,0.));
#12074=DIRECTION('ref_axis',(0.,1.,0.));
#12075=DIRECTION('',(-1.,0.,0.));
#12076=DIRECTION('center_axis',(1.,0.,0.));
#12077=DIRECTION('ref_axis',(0.,1.,0.));
#12078=DIRECTION('',(-1.,0.,0.));
#12079=DIRECTION('center_axis',(1.,0.,0.));
#12080=DIRECTION('ref_axis',(0.,1.,0.));
#12081=DIRECTION('',(-1.,0.,0.));
#12082=DIRECTION('center_axis',(1.,0.,0.));
#12083=DIRECTION('ref_axis',(0.,1.,0.));
#12084=DIRECTION('',(-1.,0.,0.));
#12085=DIRECTION('center_axis',(1.,0.,0.));
#12086=DIRECTION('ref_axis',(0.,1.,0.));
#12087=DIRECTION('',(-1.,0.,0.));
#12088=DIRECTION('center_axis',(1.,0.,0.));
#12089=DIRECTION('ref_axis',(0.,1.,0.));
#12090=DIRECTION('',(-1.,0.,0.));
#12091=DIRECTION('center_axis',(1.,0.,0.));
#12092=DIRECTION('ref_axis',(0.,-0.160289682943514,-0.987070016534728));
#12093=DIRECTION('',(1.,0.,0.));
#12094=DIRECTION('center_axis',(1.,0.,0.));
#12095=DIRECTION('ref_axis',(0.,1.,7.97687035098722E-14));
#12096=DIRECTION('center_axis',(1.,0.,0.));
#12097=DIRECTION('ref_axis',(0.,1.,7.97687035098722E-14));
#12098=DIRECTION('',(1.,0.,0.));
#12099=DIRECTION('center_axis',(1.,0.,0.));
#12100=DIRECTION('ref_axis',(0.,1.,7.97687035098722E-14));
#12101=DIRECTION('',(1.,0.,0.));
#12102=DIRECTION('center_axis',(1.,0.,0.));
#12103=DIRECTION('ref_axis',(0.,1.,7.97687035098722E-14));
#12104=DIRECTION('',(1.,0.,0.));
#12105=DIRECTION('center_axis',(1.,0.,0.));
#12106=DIRECTION('ref_axis',(0.,1.,7.97687035098722E-14));
#12107=DIRECTION('',(1.,0.,0.));
#12108=DIRECTION('center_axis',(1.,0.,0.));
#12109=DIRECTION('ref_axis',(0.,1.,7.97687035098722E-14));
#12110=DIRECTION('',(1.,0.,0.));
#12111=DIRECTION('center_axis',(1.,0.,0.));
#12112=DIRECTION('ref_axis',(0.,1.,7.97687035098722E-14));
#12113=DIRECTION('',(1.,0.,0.));
#12114=DIRECTION('center_axis',(1.,0.,0.));
#12115=DIRECTION('ref_axis',(0.,1.,7.97687035098722E-14));
#12116=DIRECTION('',(1.,0.,0.));
#12117=DIRECTION('center_axis',(1.,0.,0.));
#12118=DIRECTION('ref_axis',(0.,1.,7.97687035098722E-14));
#12119=DIRECTION('',(1.,0.,0.));
#12120=DIRECTION('center_axis',(1.,0.,0.));
#12121=DIRECTION('ref_axis',(0.,1.,7.97687035098722E-14));
#12122=DIRECTION('',(1.,0.,0.));
#12123=DIRECTION('center_axis',(1.,0.,0.));
#12124=DIRECTION('ref_axis',(0.,1.,7.97687035098722E-14));
#12125=DIRECTION('',(1.,0.,0.));
#12126=DIRECTION('center_axis',(1.,0.,0.));
#12127=DIRECTION('ref_axis',(0.,1.,7.97687035098722E-14));
#12128=DIRECTION('',(1.,0.,0.));
#12129=DIRECTION('center_axis',(1.,0.,0.));
#12130=DIRECTION('ref_axis',(0.,0.,-1.));
#12131=DIRECTION('center_axis',(1.,0.,0.));
#12132=DIRECTION('ref_axis',(0.,1.,0.));
#12133=DIRECTION('center_axis',(1.,0.,0.));
#12134=DIRECTION('ref_axis',(0.,1.,0.));
#12135=DIRECTION('center_axis',(1.,0.,0.));
#12136=DIRECTION('ref_axis',(0.,0.,-1.));
#12137=DIRECTION('center_axis',(1.,0.,0.));
#12138=DIRECTION('ref_axis',(0.,1.,0.));
#12139=DIRECTION('center_axis',(1.,0.,0.));
#12140=DIRECTION('ref_axis',(0.,1.,0.));
#12141=DIRECTION('center_axis',(-1.,0.,0.));
#12142=DIRECTION('ref_axis',(0.,1.,7.97687035098722E-14));
#12143=DIRECTION('center_axis',(1.,0.,0.));
#12144=DIRECTION('ref_axis',(0.,1.,7.97687035098722E-14));
#12145=DIRECTION('center_axis',(1.,0.,0.));
#12146=DIRECTION('ref_axis',(0.,1.,0.));
#12147=DIRECTION('',(0.521294361252099,-0.853376932502142,-1.04508532885494E-16));
#12148=DIRECTION('center_axis',(-1.,0.,0.));
#12149=DIRECTION('ref_axis',(0.,1.,0.));
#12150=DIRECTION('center_axis',(0.,0.5,0.866025403784439));
#12151=DIRECTION('ref_axis',(0.,0.866025403784439,-0.5));
#12152=DIRECTION('',(0.,0.866025403784439,-0.5));
#12153=DIRECTION('',(-1.,0.,0.));
#12154=DIRECTION('',(0.,0.866025403784439,-0.5));
#12155=DIRECTION('',(-1.,0.,0.));
#12156=DIRECTION('center_axis',(0.,-0.5,0.866025403784439));
#12157=DIRECTION('ref_axis',(0.,0.866025403784439,0.5));
#12158=DIRECTION('',(0.,0.866025403784439,0.5));
#12159=DIRECTION('',(-1.,0.,0.));
#12160=DIRECTION('',(0.,0.866025403784439,0.5));
#12161=DIRECTION('center_axis',(0.,-1.,-1.20185167898973E-16));
#12162=DIRECTION('ref_axis',(0.,-1.20185167898973E-16,1.));
#12163=DIRECTION('',(0.,-1.20185167898973E-16,1.));
#12164=DIRECTION('',(-1.,0.,0.));
#12165=DIRECTION('',(0.,-1.20185167898973E-16,1.));
#12166=DIRECTION('center_axis',(0.,-0.5,-0.866025403784439));
#12167=DIRECTION('ref_axis',(0.,-0.866025403784439,0.5));
#12168=DIRECTION('',(0.,-0.866025403784439,0.5));
#12169=DIRECTION('',(-1.,0.,0.));
#12170=DIRECTION('',(0.,-0.866025403784439,0.5));
#12171=DIRECTION('center_axis',(0.,0.5,-0.866025403784439));
#12172=DIRECTION('ref_axis',(0.,-0.866025403784439,-0.5));
#12173=DIRECTION('',(0.,-0.866025403784439,-0.5));
#12174=DIRECTION('',(-1.,0.,0.));
#12175=DIRECTION('',(0.,-0.866025403784439,-0.5));
#12176=DIRECTION('center_axis',(0.,1.,-3.60555503696918E-16));
#12177=DIRECTION('ref_axis',(0.,-3.60555503696918E-16,-1.));
#12178=DIRECTION('',(0.,-3.60555503696918E-16,-1.));
#12179=DIRECTION('',(0.,-3.60555503696918E-16,-1.));
#12180=DIRECTION('center_axis',(-1.,0.,0.));
#12181=DIRECTION('ref_axis',(0.,0.,1.));
#12182=DIRECTION('center_axis',(-1.,0.,0.));
#12183=DIRECTION('ref_axis',(0.,0.,1.));
#12184=DIRECTION('center_axis',(1.,0.,0.));
#12185=DIRECTION('ref_axis',(0.,0.,-1.));
#12186=DIRECTION('center_axis',(1.,0.,0.));
#12187=DIRECTION('ref_axis',(0.,1.,0.));
#12188=DIRECTION('',(-0.707106781186548,0.707106781186547,8.65956056235493E-17));
#12189=DIRECTION('center_axis',(1.,0.,0.));
#12190=DIRECTION('ref_axis',(0.,0.969617468264477,-0.244626174471142));
#12191=DIRECTION('center_axis',(1.,0.,0.));
#12192=DIRECTION('ref_axis',(0.,1.,0.));
#12193=DIRECTION('center_axis',(1.,0.,0.));
#12194=DIRECTION('ref_axis',(0.,1.,0.));
#12195=DIRECTION('center_axis',(1.,0.,0.));
#12196=DIRECTION('ref_axis',(0.,0.,-1.));
#12197=DIRECTION('',(-0.707106781186548,0.707106781186548,8.65956056235494E-17));
#12198=DIRECTION('center_axis',(1.,0.,0.));
#12199=DIRECTION('ref_axis',(0.,0.,-1.));
#12200=DIRECTION('axis',(0.,0.,1.));
#12201=DIRECTION('refdir',(1.,0.,0.));
#12202=DIRECTION('center_axis',(-1.,0.,0.));
#12203=DIRECTION('ref_axis',(0.,0.,1.));
#12204=DIRECTION('center_axis',(1.,0.,0.));
#12205=DIRECTION('ref_axis',(0.,0.,-1.));
#12206=DIRECTION('center_axis',(1.,0.,0.));
#12207=DIRECTION('ref_axis',(0.,1.,0.));
#12208=DIRECTION('center_axis',(1.,0.,0.));
#12209=DIRECTION('ref_axis',(0.,0.,-1.));
#12210=DIRECTION('',(-0.707106781186548,0.707106781186547,8.65956056235493E-17));
#12211=DIRECTION('center_axis',(1.,0.,0.));
#12212=DIRECTION('ref_axis',(0.,1.,0.));
#12213=DIRECTION('center_axis',(1.,0.,0.));
#12214=DIRECTION('ref_axis',(0.,0.,-1.));
#12215=DIRECTION('',(-1.,0.,0.));
#12216=DIRECTION('center_axis',(-1.,0.,0.));
#12217=DIRECTION('ref_axis',(0.,1.,0.));
#12218=DIRECTION('center_axis',(1.,0.,0.));
#12219=DIRECTION('ref_axis',(0.,0.,-1.));
#12220=DIRECTION('',(-0.707106781186546,-0.707106781186549,-8.65956056235495E-17));
#12221=DIRECTION('center_axis',(1.,0.,0.));
#12222=DIRECTION('ref_axis',(0.,0.,-1.));
#12223=DIRECTION('',(0.,0.,1.));
#12224=DIRECTION('',(1.,0.,0.));
#12225=DIRECTION('',(0.,0.,1.));
#12226=DIRECTION('',(1.,0.,0.));
#12227=DIRECTION('',(0.,0.,1.));
#12228=DIRECTION('',(1.,0.,0.));
#12229=DIRECTION('',(0.,0.,1.));
#12230=DIRECTION('',(1.,0.,0.));
#12231=DIRECTION('',(0.,0.,1.));
#12232=DIRECTION('',(1.,0.,0.));
#12233=DIRECTION('',(0.,0.,1.));
#12234=DIRECTION('',(-1.,0.,0.));
#12235=DIRECTION('',(0.,-1.66533453693773E-16,1.));
#12236=DIRECTION('',(1.,0.,0.));
#12237=DIRECTION('',(0.,-1.66533453693773E-16,1.));
#12238=DIRECTION('',(1.,0.,0.));
#12239=DIRECTION('',(0.,-1.66533453693773E-16,1.));
#12240=DIRECTION('',(1.,0.,0.));
#12241=DIRECTION('',(0.,0.,1.));
#12242=DIRECTION('',(1.,0.,0.));
#12243=DIRECTION('',(0.,0.,-1.));
#12244=DIRECTION('',(-1.,0.,0.));
#12245=DIRECTION('',(0.,-1.66533453693773E-16,1.));
#12246=DIRECTION('',(-1.,0.,0.));
#12247=DIRECTION('',(0.,1.,1.66533453693773E-16));
#12248=DIRECTION('',(0.,-1.66533453693773E-16,1.));
#12249=DIRECTION('',(0.,0.,1.));
#12250=DIRECTION('',(-1.,0.,0.));
#12251=DIRECTION('',(0.,0.,1.));
#12252=DIRECTION('',(1.,0.,0.));
#12253=DIRECTION('',(0.,0.,1.));
#12254=DIRECTION('',(-1.,0.,0.));
#12255=DIRECTION('',(0.,0.,1.));
#12256=DIRECTION('',(1.,0.,0.));
#12257=DIRECTION('',(0.,0.,1.));
#12258=DIRECTION('',(-1.,0.,0.));
#12259=DIRECTION('',(0.,0.,1.));
#12260=DIRECTION('',(1.,0.,0.));
#12261=DIRECTION('',(0.,0.,1.));
#12262=DIRECTION('',(-1.,0.,0.));
#12263=DIRECTION('',(0.,0.,1.));
#12264=DIRECTION('',(1.,0.,0.));
#12265=DIRECTION('',(0.,0.,1.));
#12266=DIRECTION('',(0.,1.,0.));
#12267=DIRECTION('',(0.,0.,1.));
#12268=DIRECTION('',(0.,1.,0.));
#12269=DIRECTION('',(0.,0.,1.));
#12270=DIRECTION('',(0.,1.,0.));
#12271=CARTESIAN_POINT('',(0.,0.,0.));
#12272=CARTESIAN_POINT('',(0.,0.,0.));
#12273=CARTESIAN_POINT('Origin',(99.75,3.15,15.85));
#12274=CARTESIAN_POINT('',(99.75,2.9,15.6));
#12275=CARTESIAN_POINT('',(100.,2.9,15.85));
#12276=CARTESIAN_POINT('',(99.75,2.9,15.6));
#12277=CARTESIAN_POINT('',(99.75,3.15,15.85));
#12278=CARTESIAN_POINT('',(99.75,3.15,15.85));
#12279=CARTESIAN_POINT('',(100.,2.9,15.85));
#12280=CARTESIAN_POINT('Origin',(0.,2.9,15.85));
#12281=CARTESIAN_POINT('',(0.25,2.9,15.6));
#12282=CARTESIAN_POINT('',(0.25,3.15,15.85));
#12283=CARTESIAN_POINT('',(0.25,2.9,15.6));
#12284=CARTESIAN_POINT('',(0.,2.9,15.85));
#12285=CARTESIAN_POINT('',(0.,2.9,15.85));
#12286=CARTESIAN_POINT('',(0.25,3.15,15.85));
#12287=CARTESIAN_POINT('Origin',(99.75,-2.9,15.6));
#12288=CARTESIAN_POINT('',(99.75,-3.15,15.85));
#12289=CARTESIAN_POINT('',(100.,-2.9,15.85));
#12290=CARTESIAN_POINT('',(99.75,-3.15,15.85));
#12291=CARTESIAN_POINT('',(99.75,-2.9,15.6));
#12292=CARTESIAN_POINT('',(99.75,-2.9,15.6));
#12293=CARTESIAN_POINT('',(100.,-2.9,15.85));
#12294=CARTESIAN_POINT('Origin',(0.,-2.9,15.85));
#12295=CARTESIAN_POINT('',(0.25,-3.15,15.85));
#12296=CARTESIAN_POINT('',(0.25,-2.9,15.6));
#12297=CARTESIAN_POINT('',(0.25,-3.15,15.85));
#12298=CARTESIAN_POINT('',(0.,-2.9,15.85));
#12299=CARTESIAN_POINT('',(0.,-2.9,15.85));
#12300=CARTESIAN_POINT('',(0.25,-2.9,15.6));
#12301=CARTESIAN_POINT('Origin',(0.125,-3.025,31.275));
#12302=CARTESIAN_POINT('',(0.25,-3.15,33.8589773110664));
#12303=CARTESIAN_POINT('',(0.,-2.9,33.8036501212914));
#12304=CARTESIAN_POINT('Origin',(-2.9,0.,47.5));
#12305=CARTESIAN_POINT('',(0.,-2.9,31.275));
#12306=CARTESIAN_POINT('',(0.25,-3.15,31.275));
#12307=CARTESIAN_POINT('Origin',(0.125,-1.575,15.725));
#12308=CARTESIAN_POINT('',(0.25,-1.575,15.6));
#12309=CARTESIAN_POINT('',(0.,-1.575,15.85));
#12310=CARTESIAN_POINT('Origin',(0.,-3.025,15.725));
#12311=CARTESIAN_POINT('',(0.,-3.15,15.85));
#12312=CARTESIAN_POINT('',(0.,-2.9,15.6));
#12313=CARTESIAN_POINT('Origin',(99.875,-1.575,15.725));
#12314=CARTESIAN_POINT('',(100.,-1.575,15.85));
#12315=CARTESIAN_POINT('',(99.75,-1.575,15.6));
#12316=CARTESIAN_POINT('Origin',(99.875,-3.025,31.275));
#12317=CARTESIAN_POINT('',(100.,-2.9,33.8036501212914));
#12318=CARTESIAN_POINT('',(99.75,-3.15,33.8589773110664));
#12319=CARTESIAN_POINT('Origin',(102.9,0.,47.5));
#12320=CARTESIAN_POINT('',(99.75,-3.15,31.275));
#12321=CARTESIAN_POINT('',(100.,-2.9,31.275));
#12322=CARTESIAN_POINT('Origin',(0.125,3.025,20.825));
#12323=CARTESIAN_POINT('',(0.,2.9,33.8036501212914));
#12324=CARTESIAN_POINT('',(0.25,3.15,33.8589773110664));
#12325=CARTESIAN_POINT('Origin',(-2.9,0.,47.5));
#12326=CARTESIAN_POINT('',(0.25,3.15,20.825));
#12327=CARTESIAN_POINT('',(0.,2.9,20.825));
#12328=CARTESIAN_POINT('Origin',(0.,3.025,15.725));
#12329=CARTESIAN_POINT('',(0.,2.9,15.6));
#12330=CARTESIAN_POINT('',(0.,3.15,15.85));
#12331=CARTESIAN_POINT('Origin',(99.875,3.025,20.825));
#12332=CARTESIAN_POINT('',(99.75,3.15,33.8589773110664));
#12333=CARTESIAN_POINT('',(100.,2.9,33.8036501212914));
#12334=CARTESIAN_POINT('Origin',(102.9,0.,47.5));
#12335=CARTESIAN_POINT('',(100.,2.9,20.825));
#12336=CARTESIAN_POINT('',(99.75,3.15,20.825));
#12337=CARTESIAN_POINT('Origin',(0.,-3.15,36.5));
#12338=CARTESIAN_POINT('',(0.,-3.15,33.8589773110664));
#12339=CARTESIAN_POINT('',(77.5,-3.15,19.));
#12340=CARTESIAN_POINT('Origin',(80.,-3.15,19.));
#12341=CARTESIAN_POINT('',(47.5,-3.15,19.));
#12342=CARTESIAN_POINT('Origin',(50.,-3.15,19.));
#12343=CARTESIAN_POINT('',(17.5,-3.15,19.));
#12344=CARTESIAN_POINT('Origin',(20.,-3.15,19.));
#12345=CARTESIAN_POINT('Origin',(100.,0.,26.05));
#12346=CARTESIAN_POINT('Origin',(100.,0.,47.5));
#12347=CARTESIAN_POINT('Origin',(0.,-3.15,15.6));
#12348=CARTESIAN_POINT('Origin',(20.,3.15,19.));
#12349=CARTESIAN_POINT('',(17.5,3.15,19.));
#12350=CARTESIAN_POINT('Origin',(20.,3.15,19.));
#12351=CARTESIAN_POINT('',(17.5,3.15,19.));
#12352=CARTESIAN_POINT('Origin',(50.,3.15,19.));
#12353=CARTESIAN_POINT('',(47.5,3.15,19.));
#12354=CARTESIAN_POINT('Origin',(50.,3.15,19.));
#12355=CARTESIAN_POINT('',(47.5,3.15,19.));
#12356=CARTESIAN_POINT('Origin',(80.,3.15,19.));
#12357=CARTESIAN_POINT('',(77.5,3.15,19.));
#12358=CARTESIAN_POINT('Origin',(80.,3.15,19.));
#12359=CARTESIAN_POINT('',(77.5,3.15,19.));
#12360=CARTESIAN_POINT('Origin',(0.,0.,47.5));
#12361=CARTESIAN_POINT('',(0.,3.15,33.8589773110664));
#12362=CARTESIAN_POINT('Origin',(0.,0.,47.5));
#12363=CARTESIAN_POINT('Origin',(0.,0.,26.05));
#12364=CARTESIAN_POINT('Origin',(0.,3.15,15.6));
#12365=CARTESIAN_POINT('',(0.,0.,0.));
#12366=CARTESIAN_POINT('Origin',(99.75,-3.15,70.25));
#12367=CARTESIAN_POINT('',(99.75,-2.9,70.5));
#12368=CARTESIAN_POINT('',(100.,-2.9,70.25));
#12369=CARTESIAN_POINT('',(99.75,-2.9,70.5));
#12370=CARTESIAN_POINT('',(99.75,-3.15,70.25));
#12371=CARTESIAN_POINT('',(99.75,-3.15,70.25));
#12372=CARTESIAN_POINT('',(100.,-2.9,70.25));
#12373=CARTESIAN_POINT('Origin',(0.25,-3.15,70.25));
#12374=CARTESIAN_POINT('',(0.,-2.9,70.25));
#12375=CARTESIAN_POINT('',(0.25,-2.9,70.5));
#12376=CARTESIAN_POINT('',(0.,-2.9,70.25));
#12377=CARTESIAN_POINT('',(0.25,-3.15,70.25));
#12378=CARTESIAN_POINT('',(0.25,-3.15,70.25));
#12379=CARTESIAN_POINT('',(0.25,-2.9,70.5));
#12380=CARTESIAN_POINT('Origin',(0.125,-3.025,67.5));
#12381=CARTESIAN_POINT('',(0.,-2.9,61.1963498787086));
#12382=CARTESIAN_POINT('',(0.25,-3.15,61.1410226889336));
#12383=CARTESIAN_POINT('Origin',(-2.9,0.,47.5));
#12384=CARTESIAN_POINT('',(0.25,-3.15,67.5));
#12385=CARTESIAN_POINT('',(0.,-2.9,67.5));
#12386=CARTESIAN_POINT('Origin',(0.,-3.025,70.375));
#12387=CARTESIAN_POINT('',(0.,-2.9,70.5));
#12388=CARTESIAN_POINT('',(0.,-3.15,70.25));
#12389=CARTESIAN_POINT('Origin',(99.75,2.9,70.5));
#12390=CARTESIAN_POINT('',(99.75,3.15,70.25));
#12391=CARTESIAN_POINT('',(100.,2.9,70.25));
#12392=CARTESIAN_POINT('',(99.75,3.15,70.25));
#12393=CARTESIAN_POINT('',(99.75,2.9,70.5));
#12394=CARTESIAN_POINT('',(99.75,2.9,70.5));
#12395=CARTESIAN_POINT('',(100.,2.9,70.25));
#12396=CARTESIAN_POINT('Origin',(0.,2.9,70.25));
#12397=CARTESIAN_POINT('',(0.25,3.15,70.25));
#12398=CARTESIAN_POINT('',(0.25,2.9,70.5));
#12399=CARTESIAN_POINT('',(0.25,3.15,70.25));
#12400=CARTESIAN_POINT('',(0.,2.9,70.25));
#12401=CARTESIAN_POINT('',(0.,2.9,70.25));
#12402=CARTESIAN_POINT('',(0.25,2.9,70.5));
#12403=CARTESIAN_POINT('Origin',(0.125,3.025,61.5));
#12404=CARTESIAN_POINT('',(0.25,3.15,61.1410226889336));
#12405=CARTESIAN_POINT('',(0.,2.9,61.1963498787086));
#12406=CARTESIAN_POINT('Origin',(-2.9,0.,47.5));
#12407=CARTESIAN_POINT('',(0.,2.9,61.5));
#12408=CARTESIAN_POINT('',(0.25,3.15,61.5));
#12409=CARTESIAN_POINT('Origin',(0.125,1.575,70.375));
#12410=CARTESIAN_POINT('',(0.25,1.575,70.5));
#12411=CARTESIAN_POINT('',(0.,1.575,70.25));
#12412=CARTESIAN_POINT('Origin',(0.,3.025,70.375));
#12413=CARTESIAN_POINT('',(0.,3.15,70.25));
#12414=CARTESIAN_POINT('',(0.,2.9,70.5));
#12415=CARTESIAN_POINT('Origin',(99.875,1.575,70.375));
#12416=CARTESIAN_POINT('',(100.,1.575,70.25));
#12417=CARTESIAN_POINT('',(99.75,1.575,70.5));
#12418=CARTESIAN_POINT('Origin',(99.875,3.025,61.5));
#12419=CARTESIAN_POINT('',(100.,2.9,61.1963498787086));
#12420=CARTESIAN_POINT('',(99.75,3.15,61.1410226889336));
#12421=CARTESIAN_POINT('Origin',(102.9,0.,47.5));
#12422=CARTESIAN_POINT('',(99.75,3.15,61.5));
#12423=CARTESIAN_POINT('',(100.,2.9,61.5));
#12424=CARTESIAN_POINT('Origin',(99.875,-3.025,67.5));
#12425=CARTESIAN_POINT('',(99.75,-3.15,61.1410226889336));
#12426=CARTESIAN_POINT('',(100.,-2.9,61.1963498787086));
#12427=CARTESIAN_POINT('Origin',(102.9,0.,47.5));
#12428=CARTESIAN_POINT('',(100.,-2.9,67.5));
#12429=CARTESIAN_POINT('',(99.75,-3.15,67.5));
#12430=CARTESIAN_POINT('Origin',(0.,3.15,58.5));
#12431=CARTESIAN_POINT('',(0.,3.15,61.1410226889336));
#12432=CARTESIAN_POINT('Origin',(100.,0.,64.5));
#12433=CARTESIAN_POINT('Origin',(100.,0.,47.5));
#12434=CARTESIAN_POINT('Origin',(0.,3.15,70.5));
#12435=CARTESIAN_POINT('Origin',(0.,0.,47.5));
#12436=CARTESIAN_POINT('',(0.,-3.15,61.1410226889336));
#12437=CARTESIAN_POINT('Origin',(0.,0.,47.5));
#12438=CARTESIAN_POINT('Origin',(0.,0.,64.5));
#12439=CARTESIAN_POINT('Origin',(0.,-3.15,70.5));
#12440=CARTESIAN_POINT('',(0.,0.,0.));
#12441=CARTESIAN_POINT('Origin',(-0.1,29.,58.575));
#12442=CARTESIAN_POINT('',(-0.2,29.1,66.6));
#12443=CARTESIAN_POINT('',(0.,28.9,66.6));
#12444=CARTESIAN_POINT('',(-0.2,29.1,66.6));
#12445=CARTESIAN_POINT('',(0.,28.9,26.5));
#12446=CARTESIAN_POINT('',(0.,28.9,58.575));
#12447=CARTESIAN_POINT('',(-0.2,29.1,26.5));
#12448=CARTESIAN_POINT('',(0.,28.9,26.5));
#12449=CARTESIAN_POINT('',(-0.2,29.1,58.575));
#12450=CARTESIAN_POINT('Origin',(-0.1,25.1,66.6));
#12451=CARTESIAN_POINT('',(-0.2,25.1,70.6));
#12452=CARTESIAN_POINT('Origin',(-0.2,25.1,66.6));
#12453=CARTESIAN_POINT('',(0.,25.1,70.4));
#12454=CARTESIAN_POINT('',(-0.2,25.1,70.6));
#12455=CARTESIAN_POINT('Origin',(0.,25.1,66.6));
#12456=CARTESIAN_POINT('Origin',(-0.1,-14.55,70.5));
#12457=CARTESIAN_POINT('',(-0.2,-25.1,70.6));
#12458=CARTESIAN_POINT('',(0.,-25.1,70.4));
#12459=CARTESIAN_POINT('',(-0.2,-25.1,70.6));
#12460=CARTESIAN_POINT('',(0.,-14.55,70.4));
#12461=CARTESIAN_POINT('',(-0.2,-14.55,70.6));
#12462=CARTESIAN_POINT('Origin',(-0.1,-25.1,66.6));
#12463=CARTESIAN_POINT('',(-0.2,-29.1,66.6));
#12464=CARTESIAN_POINT('Origin',(-0.2,-25.1,66.6));
#12465=CARTESIAN_POINT('',(0.,-28.9,66.6));
#12466=CARTESIAN_POINT('',(-0.2,-29.1,66.6));
#12467=CARTESIAN_POINT('Origin',(0.,-25.1,66.6));
#12468=CARTESIAN_POINT('Origin',(-0.1,-29.,34.525));
#12469=CARTESIAN_POINT('',(-0.2,-29.1,26.5));
#12470=CARTESIAN_POINT('',(0.,-28.9,26.5));
#12471=CARTESIAN_POINT('',(-0.2,-29.1,26.5));
#12472=CARTESIAN_POINT('',(0.,-28.9,34.525));
#12473=CARTESIAN_POINT('',(-0.2,-29.1,34.525));
#12474=CARTESIAN_POINT('Origin',(-0.1,-25.1,26.5));
#12475=CARTESIAN_POINT('',(-0.2,-25.1,22.5));
#12476=CARTESIAN_POINT('Origin',(-0.2,-25.1,26.5));
#12477=CARTESIAN_POINT('',(0.,-25.1,22.7));
#12478=CARTESIAN_POINT('',(-0.2,-25.1,22.5));
#12479=CARTESIAN_POINT('Origin',(0.,-25.1,26.5));
#12480=CARTESIAN_POINT('Origin',(-0.1,14.55,22.6));
#12481=CARTESIAN_POINT('',(-0.2,25.1,22.5));
#12482=CARTESIAN_POINT('',(0.,25.1,22.7));
#12483=CARTESIAN_POINT('',(-0.2,25.1,22.5));
#12484=CARTESIAN_POINT('',(0.,14.55,22.7));
#12485=CARTESIAN_POINT('',(-0.2,14.55,22.5));
#12486=CARTESIAN_POINT('Origin',(-0.1,25.1,26.5));
#12487=CARTESIAN_POINT('Origin',(-0.2,25.1,26.5));
#12488=CARTESIAN_POINT('Origin',(0.,25.1,26.5));
#12489=CARTESIAN_POINT('Origin',(0.,-25.1,66.6));
#12490=CARTESIAN_POINT('',(-2.3,-25.1,70.6));
#12491=CARTESIAN_POINT('',(0.,-25.1,70.6));
#12492=CARTESIAN_POINT('',(-2.3,-29.1,66.6));
#12493=CARTESIAN_POINT('Origin',(-2.3,-25.1,66.6));
#12494=CARTESIAN_POINT('',(0.,-29.1,66.6));
#12495=CARTESIAN_POINT('Origin',(0.,-29.1,70.6));
#12496=CARTESIAN_POINT('',(-2.3,25.1,70.6));
#12497=CARTESIAN_POINT('',(0.,25.1,70.6));
#12498=CARTESIAN_POINT('',(-2.3,-21.825,70.6));
#12499=CARTESIAN_POINT('Origin',(0.,25.1,66.6));
#12500=CARTESIAN_POINT('',(-2.3,29.1,66.6));
#12501=CARTESIAN_POINT('',(0.,29.1,66.6));
#12502=CARTESIAN_POINT('Origin',(-2.3,25.1,66.6));
#12503=CARTESIAN_POINT('Origin',(0.,29.1,70.6));
#12504=CARTESIAN_POINT('',(-2.3,29.1,26.5));
#12505=CARTESIAN_POINT('',(0.,29.1,26.5));
#12506=CARTESIAN_POINT('',(-2.3,29.1,64.5875));
#12507=CARTESIAN_POINT('Origin',(0.,0.,46.55));
#12508=CARTESIAN_POINT('',(0.,25.,28.2));
#12509=CARTESIAN_POINT('Origin',(0.,25.,26.5));
#12510=CARTESIAN_POINT('',(0.,-25.,68.2));
#12511=CARTESIAN_POINT('Origin',(0.,-25.,66.5));
#12512=CARTESIAN_POINT('',(0.,-25.,28.2));
#12513=CARTESIAN_POINT('Origin',(0.,-25.,26.5));
#12514=CARTESIAN_POINT('',(0.,25.,68.2));
#12515=CARTESIAN_POINT('Origin',(0.,25.,66.5));
#12516=CARTESIAN_POINT('',(0.,7.9602041944578E-16,54.));
#12517=CARTESIAN_POINT('Origin',(0.,0.,47.5));
#12518=CARTESIAN_POINT('Origin',(-2.47071067811866,-29.0292893218814,28.5125));
#12519=CARTESIAN_POINT('',(-2.64142135623731,-28.9585786437627,66.6));
#12520=CARTESIAN_POINT('',(-2.3,-29.1,66.6));
#12521=CARTESIAN_POINT('',(-2.64142135623731,-28.9585786437627,26.5));
#12522=CARTESIAN_POINT('',(-2.64142135623731,-28.9585786437627,28.5125));
#12523=CARTESIAN_POINT('',(-2.3,-29.1,26.5));
#12524=CARTESIAN_POINT('',(-2.64142135623731,-28.9585786437627,26.5));
#12525=CARTESIAN_POINT('',(-2.3,-29.1,28.5125));
#12526=CARTESIAN_POINT('Origin',(-2.47071067811865,-25.1,66.6));
#12527=CARTESIAN_POINT('',(-2.6414213562373,-25.1,70.4585786437627));
#12528=CARTESIAN_POINT('',(-2.3,-25.1,70.6));
#12529=CARTESIAN_POINT('Origin',(-2.64142135623731,-25.1,66.6));
#12530=CARTESIAN_POINT('Origin',(-2.47071067811865,-21.825,70.5292893218814));
#12531=CARTESIAN_POINT('',(-2.64142135623731,25.1,70.4585786437627));
#12532=CARTESIAN_POINT('',(-2.3,25.1,70.6));
#12533=CARTESIAN_POINT('',(-2.64142135623731,-21.825,70.4585786437627));
#12534=CARTESIAN_POINT('Origin',(-2.47071067811865,25.1,66.6));
#12535=CARTESIAN_POINT('',(-2.64142135623731,28.9585786437627,66.6));
#12536=CARTESIAN_POINT('',(-2.3,29.1,66.6));
#12537=CARTESIAN_POINT('Origin',(-2.64142135623731,25.1,66.6));
#12538=CARTESIAN_POINT('Origin',(-2.47071067811866,29.0292893218814,64.5875));
#12539=CARTESIAN_POINT('',(-2.64142135623731,28.9585786437627,26.5));
#12540=CARTESIAN_POINT('',(-2.3,29.1,26.5));
#12541=CARTESIAN_POINT('',(-2.64142135623731,28.9585786437627,64.5875));
#12542=CARTESIAN_POINT('Origin',(-2.47071067811865,25.1,26.5));
#12543=CARTESIAN_POINT('',(-2.3,25.1,22.5));
#12544=CARTESIAN_POINT('',(-2.64142135623731,25.1,22.6414213562373));
#12545=CARTESIAN_POINT('',(-2.3,25.1,22.5));
#12546=CARTESIAN_POINT('Origin',(-2.64142135623731,25.1,26.5));
#12547=CARTESIAN_POINT('Origin',(-2.3,25.1,26.5));
#12548=CARTESIAN_POINT('Origin',(-2.47071067811866,21.825,22.5707106781187));
#12549=CARTESIAN_POINT('',(-2.61819805153193,4.14309288132937,22.6318019484637));
#12550=CARTESIAN_POINT('',(-2.64142135623725,4.14658995368148,22.6414213562372));
#12551=CARTESIAN_POINT('Ctrl Pts',(-2.61819805153193,4.14309288132937,22.6318019484637));
#12552=CARTESIAN_POINT('Ctrl Pts',(-2.6259378790126,4.14426860505579,22.6350078899766));
#12553=CARTESIAN_POINT('Ctrl Pts',(-2.63367898747496,4.14543428596151,22.638214362091));
#12554=CARTESIAN_POINT('Ctrl Pts',(-2.64142135623725,4.14658995368148,22.6414213562372));
#12555=CARTESIAN_POINT('',(-2.64142135623731,21.825,22.6414213562373));
#12556=CARTESIAN_POINT('',(-2.3,-25.1,22.5));
#12557=CARTESIAN_POINT('',(-2.3,21.825,22.5));
#12558=CARTESIAN_POINT('',(-2.64142135623731,-25.1,22.6414213562373));
#12559=CARTESIAN_POINT('',(-2.3,-25.1,22.5));
#12560=CARTESIAN_POINT('',(-2.64142135623721,1.29697164052348,22.6414213562372));
#12561=CARTESIAN_POINT('',(-2.64142135623731,21.825,22.6414213562373));
#12562=CARTESIAN_POINT('',(-2.61819805153393,1.30034092007739,22.631801948466));
#12563=CARTESIAN_POINT('Ctrl Pts',(-2.64142135623721,1.29697164052832,22.6414213562231));
#12564=CARTESIAN_POINT('Ctrl Pts',(-2.63367876608245,1.29808438048699,22.6382142703778));
#12565=CARTESIAN_POINT('Ctrl Pts',(-2.62593762971128,1.29920745199881,22.6350077867096));
#12566=CARTESIAN_POINT('Ctrl Pts',(-2.61819805153393,1.30034092007804,22.6318019484642));
#12567=CARTESIAN_POINT('',(-2.61819805153395,15.230763933342,22.6318019484661));
#12568=CARTESIAN_POINT('Origin',(-2.47071067811865,-25.1,26.5));
#12569=CARTESIAN_POINT('Origin',(-2.64142135623731,-25.1,26.5));
#12570=CARTESIAN_POINT('Origin',(-2.3,-25.1,26.5));
#12571=CARTESIAN_POINT('Origin',(0.,-29.1,22.5));
#12572=CARTESIAN_POINT('',(0.,-29.1,26.5));
#12573=CARTESIAN_POINT('Origin',(-2.75,25.1,66.6));
#12574=CARTESIAN_POINT('',(-2.85857864376269,28.7414213562373,66.6));
#12575=CARTESIAN_POINT('',(-3.,28.6,66.6));
#12576=CARTESIAN_POINT('',(-2.85857864376269,25.1,70.2414213562373));
#12577=CARTESIAN_POINT('Origin',(-2.85857864376269,25.1,66.6));
#12578=CARTESIAN_POINT('',(-3.,25.1,70.1));
#12579=CARTESIAN_POINT('Origin',(-2.75,28.85,58.575));
#12580=CARTESIAN_POINT('',(-2.85857864376269,28.7414213562373,26.5));
#12581=CARTESIAN_POINT('',(-3.,28.6,26.5));
#12582=CARTESIAN_POINT('',(-2.85857864376269,28.7414213562373,52.5625));
#12583=CARTESIAN_POINT('Origin',(-2.75,25.1,26.5));
#12584=CARTESIAN_POINT('',(-2.85857864376269,25.1,22.8585786437627));
#12585=CARTESIAN_POINT('',(-3.,25.1,23.));
#12586=CARTESIAN_POINT('Origin',(-2.85857864376269,25.1,26.5));
#12587=CARTESIAN_POINT('Origin',(-2.75,14.55,22.75));
#12588=CARTESIAN_POINT('',(-2.85857864376269,-25.1,22.8585786437627));
#12589=CARTESIAN_POINT('',(-3.,-25.1,23.));
#12590=CARTESIAN_POINT('',(-2.85857864376269,-2.52878561615944,22.8585786437627));
#12591=CARTESIAN_POINT('',(-2.85857864376269,7.275,22.8585786437627));
#12592=CARTESIAN_POINT('',(-2.75,-2.52878561615944,22.75));
#12593=CARTESIAN_POINT('',(-2.91343792378902,-2.52878561615944,22.913437923789));
#12594=CARTESIAN_POINT('',(-2.75,-2.10532046854496,22.75));
#12595=CARTESIAN_POINT('',(-2.75,5.68263995423913,22.75));
#12596=CARTESIAN_POINT('',(-2.85857864376269,-2.10532046854496,22.8585786437627));
#12597=CARTESIAN_POINT('',(-2.55000001788139,-2.10532046854496,22.5500000178814));
#12598=CARTESIAN_POINT('',(-2.85857864376269,0.201909989118576,22.8585786437627));
#12599=CARTESIAN_POINT('',(-2.85857864376269,7.275,22.8585786437627));
#12600=CARTESIAN_POINT('',(-2.75,0.201909989118576,22.75));
#12601=CARTESIAN_POINT('',(-2.91343792378902,0.201909989118576,22.913437923789));
#12602=CARTESIAN_POINT('',(-2.75,0.625375136733055,22.75));
#12603=CARTESIAN_POINT('',(-2.75,7.04798775687814,22.75));
#12604=CARTESIAN_POINT('',(-3.,0.625375136733055,23.));
#12605=CARTESIAN_POINT('',(-2.55000001788139,0.625375136733055,22.5500000178814));
#12606=CARTESIAN_POINT('',(-3.,1.21228337796395,23.));
#12607=CARTESIAN_POINT('',(-3.,14.55,23.));
#12608=CARTESIAN_POINT('',(-2.75,1.26319920824794,22.75));
#12609=CARTESIAN_POINT('Ctrl Pts',(-3.,1.21228337796395,23.));
#12610=CARTESIAN_POINT('Ctrl Pts',(-2.961213895248,1.21754813042459,22.961213895248));
#12611=CARTESIAN_POINT('Ctrl Pts',(-2.92250031201436,1.22395187924894,22.9225003120144));
#12612=CARTESIAN_POINT('Ctrl Pts',(-2.88391049622622,1.23157435155926,22.8839104962262));
#12613=CARTESIAN_POINT('Ctrl Pts',(-2.83908487466434,1.24042855446668,22.8390848746643));
#12614=CARTESIAN_POINT('Ctrl Pts',(-2.7944213152606,1.25092814815388,22.7944213152606));
#12615=CARTESIAN_POINT('Ctrl Pts',(-2.75,1.26319920824794,22.75));
#12616=CARTESIAN_POINT('Ctrl Pts',(-2.6414213562372,1.29697164052344,22.6414213562372));
#12617=CARTESIAN_POINT('Ctrl Pts',(-2.66759311479328,1.28789101002667,22.6675931147933));
#12618=CARTESIAN_POINT('Ctrl Pts',(-2.69302939122751,1.27976201495126,22.693031510606));
#12619=CARTESIAN_POINT('Ctrl Pts',(-2.71789496870931,1.27239069164872,22.7178960977404));
#12620=CARTESIAN_POINT('Ctrl Pts',(-2.72869989814678,1.26918760383774,22.7287005968387));
#12621=CARTESIAN_POINT('Ctrl Pts',(-2.73939706851147,1.26612818972238,22.7393970685115));
#12622=CARTESIAN_POINT('Ctrl Pts',(-2.75,1.26319920824794,22.75));
#12623=CARTESIAN_POINT('Origin',(-2.75,14.55,22.75));
#12624=CARTESIAN_POINT('',(-2.75,4.18187951621146,22.75));
#12625=CARTESIAN_POINT('Ctrl Pts',(-2.75,4.18187951621146,22.75));
#12626=CARTESIAN_POINT('Ctrl Pts',(-2.72593839074587,4.17489652893168,22.7259383907459));
#12627=CARTESIAN_POINT('Ctrl Pts',(-2.70113892579397,4.16715584610488,22.7011399902602));
#12628=CARTESIAN_POINT('Ctrl Pts',(-2.675415676397,4.15846008560732,22.6754162485616));
#12629=CARTESIAN_POINT('Ctrl Pts',(-2.66426294033361,4.15468989622716,22.6642632990527));
#12630=CARTESIAN_POINT('Ctrl Pts',(-2.65293655145142,4.15073955259153,22.6529365514514));
#12631=CARTESIAN_POINT('Ctrl Pts',(-2.64142135623724,4.14658995368149,22.6414213562372));
#12632=CARTESIAN_POINT('',(-2.85857864376269,4.20972540916711,22.8585786437627));
#12633=CARTESIAN_POINT('Ctrl Pts',(-2.75,4.18187951621146,22.75));
#12634=CARTESIAN_POINT('Ctrl Pts',(-2.78604207307411,4.19233938758395,22.7860420730741));
#12635=CARTESIAN_POINT('Ctrl Pts',(-2.82223699994704,4.20161368298381,22.822236999947));
#12636=CARTESIAN_POINT('Ctrl Pts',(-2.85857864376269,4.20972540916711,22.8585786437627));
#12637=CARTESIAN_POINT('',(-2.85857864376269,7.275,22.8585786437627));
#12638=CARTESIAN_POINT('Ctrl Pts',(-3.90882250993909,3.66863444045392,21.6333060643901));
#12639=CARTESIAN_POINT('Ctrl Pts',(-1.59117749006091,3.66863444045392,21.6333060643901));
#12640=CARTESIAN_POINT('Ctrl Pts',(-3.90882250993909,3.86924203284188,22.0464620601053));
#12641=CARTESIAN_POINT('Ctrl Pts',(-1.59117749006091,3.86924203284188,22.0464620601053));
#12642=CARTESIAN_POINT('Ctrl Pts',(-3.90882250993909,4.06984962522984,22.4596180558205));
#12643=CARTESIAN_POINT('Ctrl Pts',(-1.59117749006091,4.06984962522984,22.4596180558205));
#12644=CARTESIAN_POINT('Ctrl Pts',(-3.90882250993909,4.25320571288467,22.8372441768646));
#12645=CARTESIAN_POINT('Ctrl Pts',(-1.59117749006091,4.25320571288467,22.8372441768646));
#12646=CARTESIAN_POINT('Ctrl Pts',(-3.90882250993909,4.25320571288467,23.2585265278816));
#12647=CARTESIAN_POINT('Ctrl Pts',(-1.59117749006091,4.25320571288467,23.2585265278816));
#12648=CARTESIAN_POINT('Ctrl Pts',(-3.90882250993909,4.25320571288467,23.6152196445594));
#12649=CARTESIAN_POINT('Ctrl Pts',(-1.59117749006091,4.25320571288467,23.6152196445594));
#12650=CARTESIAN_POINT('Ctrl Pts',(-3.90882250993909,4.25320571288467,23.9719127612371));
#12651=CARTESIAN_POINT('Ctrl Pts',(-1.59117749006091,4.25320571288467,23.9719127612371));
#12652=CARTESIAN_POINT('',(-2.75,4.22764086327576,22.95));
#12653=CARTESIAN_POINT('Ctrl Pts',(-2.61819805153246,4.14309288132937,22.6318019484625));
#12654=CARTESIAN_POINT('Ctrl Pts',(-2.66129757451431,4.1812519561426,22.735853401377));
#12655=CARTESIAN_POINT('Ctrl Pts',(-2.705238006854,4.20937166018217,22.8419349890681));
#12656=CARTESIAN_POINT('Ctrl Pts',(-2.74999999999719,4.22764086327461,22.9499999999932));
#12657=CARTESIAN_POINT('',(-2.75,4.25320571288467,23.2585265278816));
#12658=CARTESIAN_POINT('Ctrl Pts',(-2.75,4.22764086327576,22.95));
#12659=CARTESIAN_POINT('Ctrl Pts',(-2.75,4.25320571288467,23.101219828165));
#12660=CARTESIAN_POINT('Ctrl Pts',(-2.75,4.25320571288467,23.2585265278816));
#12661=CARTESIAN_POINT('',(-3.,4.25320571288467,23.2585265278816));
#12662=CARTESIAN_POINT('',(-3.,4.25320571288467,23.2585265278816));
#12663=CARTESIAN_POINT('',(-3.,4.25231459025407,23.2));
#12664=CARTESIAN_POINT('Ctrl Pts',(-3.,4.25231459025407,23.2));
#12665=CARTESIAN_POINT('Ctrl Pts',(-3.,4.25320571288467,23.2291571778681));
#12666=CARTESIAN_POINT('Ctrl Pts',(-3.,4.25320571288467,23.2585265278816));
#12667=CARTESIAN_POINT('Ctrl Pts',(-2.85857864376269,4.20972540916711,22.8585786437626));
#12668=CARTESIAN_POINT('Ctrl Pts',(-2.87504619169403,4.21859928476957,22.8983348213176));
#12669=CARTESIAN_POINT('Ctrl Pts',(-2.89164111829844,4.22611131569154,22.9383985181925));
#12670=CARTESIAN_POINT('Ctrl Pts',(-2.90836309848014,4.23226475621148,22.9787689495369));
#12671=CARTESIAN_POINT('Ctrl Pts',(-2.93876009161904,4.24345039853569,23.0521537826282));
#12672=CARTESIAN_POINT('Ctrl Pts',(-2.96931533762918,4.25005052457576,23.1259206719475));
#12673=CARTESIAN_POINT('Ctrl Pts',(-3.,4.25231459025406,23.2));
#12674=CARTESIAN_POINT('Origin',(-2.67928932188135,8.6365278666839,22.7792893218814));
#12675=CARTESIAN_POINT('',(-2.75,1.21971470205851,22.95));
#12676=CARTESIAN_POINT('Ctrl Pts',(-2.74999999998749,1.21971470206339,22.9499999999698));
#12677=CARTESIAN_POINT('Ctrl Pts',(-2.73139877750455,1.2269752233707,22.9050926763748));
#12678=CARTESIAN_POINT('Ctrl Pts',(-2.71230553313965,1.23602156967566,22.8590058283899));
#12679=CARTESIAN_POINT('Ctrl Pts',(-2.69279642154661,1.24726736451132,22.8119079585131));
#12680=CARTESIAN_POINT('Ctrl Pts',(-2.67356362688915,1.25835387974306,22.7654771584316));
#12681=CARTESIAN_POINT('Ctrl Pts',(-2.65392666183419,1.27157792698435,22.7180637445991));
#12682=CARTESIAN_POINT('Ctrl Pts',(-2.63395849080496,1.28738081230999,22.669852665828));
#12683=CARTESIAN_POINT('Ctrl Pts',(-2.62872730492721,1.29152079240241,22.6572225098638));
#12684=CARTESIAN_POINT('Ctrl Pts',(-2.62347338787422,1.2958380073702,22.6445377370048));
#12685=CARTESIAN_POINT('Ctrl Pts',(-2.61819805153393,1.30034092007739,22.631801948466));
#12686=CARTESIAN_POINT('',(-2.75,8.6365278666839,22.95));
#12687=CARTESIAN_POINT('Origin',(-2.92928932188134,-25.,26.5));
#12688=CARTESIAN_POINT('',(-2.85857864376269,-25.,29.6085786437627));
#12689=CARTESIAN_POINT('Origin',(-2.85857864376269,-25.,26.5));
#12690=CARTESIAN_POINT('',(-3.,-25.,29.95));
#12691=CARTESIAN_POINT('',(-2.92928932188134,-25.,29.7792893218813));
#12692=CARTESIAN_POINT('',(-3.,-23.9937694101251,23.2));
#12693=CARTESIAN_POINT('Origin',(-3.,-25.,26.5));
#12694=CARTESIAN_POINT('',(-2.96924080768304,-25.1,23.1257407407407));
#12695=CARTESIAN_POINT('Ctrl Pts',(-3.,-23.9937694101251,23.2));
#12696=CARTESIAN_POINT('Ctrl Pts',(-2.96584661721312,-24.5468847050626,
23.117546440075));
#12697=CARTESIAN_POINT('Ctrl Pts',(-2.96924080768304,-25.1,23.1257407407407));
#12698=CARTESIAN_POINT('',(-2.98964466094068,-28.425,26.5));
#12699=CARTESIAN_POINT('Ctrl Pts',(-2.96924080768304,-25.1,23.1257407407407));
#12700=CARTESIAN_POINT('Ctrl Pts',(-2.97167617572008,-25.496866151748,23.1316202392852));
#12701=CARTESIAN_POINT('Ctrl Pts',(-2.97423902617588,-25.9145067633212,
23.2113907046527));
#12702=CARTESIAN_POINT('Ctrl Pts',(-2.97919487113465,-26.7221083621966,
23.5339522011638));
#12703=CARTESIAN_POINT('Ctrl Pts',(-2.98155520782326,-27.1067474485937,
23.7906699067144));
#12704=CARTESIAN_POINT('Ctrl Pts',(-2.98530798368454,-27.7182976093007,
24.3894378387628));
#12705=CARTESIAN_POINT('Ctrl Pts',(-2.98694203866927,-27.9845822543924,
24.7719850468527));
#12706=CARTESIAN_POINT('Ctrl Pts',(-2.98911037827991,-28.337933609961,25.6124281223253));
#12707=CARTESIAN_POINT('Ctrl Pts',(-2.98964466094067,-28.425,26.0703241244361));
#12708=CARTESIAN_POINT('Ctrl Pts',(-2.98964466094067,-28.425,26.5));
#12709=CARTESIAN_POINT('',(-3.,-28.4,27.0852349955359));
#12710=CARTESIAN_POINT('Ctrl Pts',(-2.98964466094068,-28.425,26.5));
#12711=CARTESIAN_POINT('Ctrl Pts',(-2.98964466094068,-28.425,26.792617497768));
#12712=CARTESIAN_POINT('Ctrl Pts',(-3.,-28.4,27.0852349955359));
#12713=CARTESIAN_POINT('Origin',(-3.,-25.,26.5));
#12714=CARTESIAN_POINT('Origin',(-2.92928932188135,-25.1,26.5));
#12715=CARTESIAN_POINT('',(-3.,-25.1,23.2));
#12716=CARTESIAN_POINT('',(-2.85857864376269,-28.7414213562373,26.5));
#12717=CARTESIAN_POINT('Origin',(-2.85857864376269,-25.1,26.5));
#12718=CARTESIAN_POINT('',(-3.,-28.4,26.5));
#12719=CARTESIAN_POINT('Origin',(-2.92928932188134,7.275,23.0292893218813));
#12720=CARTESIAN_POINT('',(-3.,-4.03055921196938,23.2));
#12721=CARTESIAN_POINT('',(-3.,7.275,23.2));
#12722=CARTESIAN_POINT('',(-2.98084332489689,-4.03055921196938,23.1537516951561));
#12723=CARTESIAN_POINT('',(-3.02322456252495,-4.03055921196938,23.2560690538279));
#12724=CARTESIAN_POINT('',(-2.98084332489689,-2.52878561615944,23.1537516951561));
#12725=CARTESIAN_POINT('',(-2.98084332489689,1.62222039401531,23.1537516951561));
#12726=CARTESIAN_POINT('',(-2.9564690384473,-2.52878561615944,23.0949069622363));
#12727=CARTESIAN_POINT('Origin',(-2.225,-25.,26.5));
#12728=CARTESIAN_POINT('',(-1.45,-25.,28.2));
#12729=CARTESIAN_POINT('',(-2.225,-25.,28.975));
#12730=CARTESIAN_POINT('Origin',(-1.45,-25.,26.5));
#12731=CARTESIAN_POINT('Origin',(-2.92928932188134,25.,26.5));
#12732=CARTESIAN_POINT('',(-2.85857864376269,25.,29.6085786437627));
#12733=CARTESIAN_POINT('Origin',(-2.85857864376269,25.,26.5));
#12734=CARTESIAN_POINT('',(-3.00000000039677,25.,29.9500000009579));
#12735=CARTESIAN_POINT('',(-2.92928932188134,25.,29.7792893218813));
#12736=CARTESIAN_POINT('',(-3.,28.4,27.0852349955359));
#12737=CARTESIAN_POINT('Origin',(-3.,25.,26.5));
#12738=CARTESIAN_POINT('',(-2.98964466094067,28.425,26.5));
#12739=CARTESIAN_POINT('Ctrl Pts',(-3.,28.4,27.0852349955359));
#12740=CARTESIAN_POINT('Ctrl Pts',(-2.98964466094067,28.425,26.792617497768));
#12741=CARTESIAN_POINT('Ctrl Pts',(-2.98964466094067,28.425,26.5));
#12742=CARTESIAN_POINT('',(-2.96924080768304,25.1,23.1257407407407));
#12743=CARTESIAN_POINT('Ctrl Pts',(-2.98964466094067,28.425,26.5));
#12744=CARTESIAN_POINT('Ctrl Pts',(-2.98964466094067,28.425,26.0703241244361));
#12745=CARTESIAN_POINT('Ctrl Pts',(-2.98911037827991,28.337933609961,25.6124281223253));
#12746=CARTESIAN_POINT('Ctrl Pts',(-2.98694203866927,27.9845822543924,24.7719850468527));
#12747=CARTESIAN_POINT('Ctrl Pts',(-2.98530798368454,27.7182976093007,24.3894378387628));
#12748=CARTESIAN_POINT('Ctrl Pts',(-2.98155520782326,27.1067474485937,23.7906699067144));
#12749=CARTESIAN_POINT('Ctrl Pts',(-2.97919487113465,26.7221083621966,23.5339522011638));
#12750=CARTESIAN_POINT('Ctrl Pts',(-2.97423902617588,25.9145067633212,23.2113907046527));
#12751=CARTESIAN_POINT('Ctrl Pts',(-2.97167617572009,25.496866151748,23.1316202392852));
#12752=CARTESIAN_POINT('Ctrl Pts',(-2.96924080768304,25.1,23.1257407407407));
#12753=CARTESIAN_POINT('',(-3.,23.9937694101251,23.2));
#12754=CARTESIAN_POINT('Ctrl Pts',(-2.96924080768304,25.1,23.1257407407407));
#12755=CARTESIAN_POINT('Ctrl Pts',(-2.96584661719341,24.5468847018497,23.1175464400274));
#12756=CARTESIAN_POINT('Ctrl Pts',(-3.00000000039677,23.9937694036995,23.2000000009579));
#12757=CARTESIAN_POINT('Origin',(-3.,25.,26.5));
#12758=CARTESIAN_POINT('Origin',(-2.92928932188135,25.1,26.5));
#12759=CARTESIAN_POINT('',(-3.,28.4,26.5));
#12760=CARTESIAN_POINT('',(-3.,25.1,23.2));
#12761=CARTESIAN_POINT('Origin',(-2.92928932188134,28.5707106781187,52.5625));
#12762=CARTESIAN_POINT('',(-3.,28.4,65.9147650044641));
#12763=CARTESIAN_POINT('',(-3.,28.4,52.5625));
#12764=CARTESIAN_POINT('',(-2.98994700660664,28.4242700729927,66.6));
#12765=CARTESIAN_POINT('Ctrl Pts',(-2.98994700660664,28.4242700729927,66.6));
#12766=CARTESIAN_POINT('Ctrl Pts',(-2.98787522829607,28.4292717882883,66.2573825022345));
#12767=CARTESIAN_POINT('Ctrl Pts',(-3.,28.4,65.9147650044641));
#12768=CARTESIAN_POINT('',(-3.,28.4,66.6));
#12769=CARTESIAN_POINT('Origin',(-2.225,25.,26.5));
#12770=CARTESIAN_POINT('',(-1.45,25.,28.2));
#12771=CARTESIAN_POINT('',(-2.225,25.,28.975));
#12772=CARTESIAN_POINT('Origin',(-1.45,25.,26.5));
#12773=CARTESIAN_POINT('Origin',(-2.92928932188134,-25.,66.5));
#12774=CARTESIAN_POINT('',(-2.85857864376269,-25.,69.6085786437627));
#12775=CARTESIAN_POINT('Origin',(-2.85857864376269,-25.,66.5));
#12776=CARTESIAN_POINT('',(-2.9896446609407,-25.,69.9249999999999));
#12777=CARTESIAN_POINT('',(-2.92928932188134,-25.,69.7792893218814));
#12778=CARTESIAN_POINT('',(-3.,-24.4147650044641,69.9));
#12779=CARTESIAN_POINT('Ctrl Pts',(-2.9896446609407,-25.,69.9249999999999));
#12780=CARTESIAN_POINT('Ctrl Pts',(-2.98964466094078,-24.7073825022338,
69.9249999999997));
#12781=CARTESIAN_POINT('Ctrl Pts',(-3.,-24.4147650044641,69.9));
#12782=CARTESIAN_POINT('',(-3.,-28.4,65.9147650044641));
#12783=CARTESIAN_POINT('Origin',(-3.,-25.,66.5));
#12784=CARTESIAN_POINT('',(-2.98994700660664,-28.4242700729927,66.6));
#12785=CARTESIAN_POINT('Ctrl Pts',(-3.,-28.4,65.9147650044641));
#12786=CARTESIAN_POINT('Ctrl Pts',(-2.98787522829607,-28.4292717882883,
66.2573825022345));
#12787=CARTESIAN_POINT('Ctrl Pts',(-2.98994700660664,-28.4242700729927,
66.6));
#12788=CARTESIAN_POINT('',(-2.98994700660664,-25.1,69.9242700729927));
#12789=CARTESIAN_POINT('Ctrl Pts',(-2.98994700660664,-28.4242700729927,
66.6));
#12790=CARTESIAN_POINT('Ctrl Pts',(-2.99238240184869,-28.4183905087696,
67.0027501492822));
#12791=CARTESIAN_POINT('Ctrl Pts',(-2.99447851800497,-28.3364130892601,
67.4263094322197));
#12792=CARTESIAN_POINT('Ctrl Pts',(-2.99745891948881,-28.0052855480682,
68.2431214573392));
#12793=CARTESIAN_POINT('Ctrl Pts',(-2.99822330470336,-27.7420564500924,
68.6309143229168));
#12794=CARTESIAN_POINT('Ctrl Pts',(-2.99822330470336,-27.1309143229168,
69.2420564500924));
#12795=CARTESIAN_POINT('Ctrl Pts',(-2.99745891948882,-26.7431214573392,
69.5052855480682));
#12796=CARTESIAN_POINT('Ctrl Pts',(-2.99447851800497,-25.9263094322197,
69.8364130892601));
#12797=CARTESIAN_POINT('Ctrl Pts',(-2.99238240184869,-25.5027501492822,
69.9183905087696));
#12798=CARTESIAN_POINT('Ctrl Pts',(-2.98994700660664,-25.1,69.9242700729927));
#12799=CARTESIAN_POINT('Ctrl Pts',(-2.98994700660664,-25.1,69.9242700729927));
#12800=CARTESIAN_POINT('Ctrl Pts',(-2.98964466094069,-25.05,69.925));
#12801=CARTESIAN_POINT('Ctrl Pts',(-2.9896446609407,-25.,69.9249999999999));
#12802=CARTESIAN_POINT('Origin',(-2.92928932188134,-28.5707106781187,40.5375));
#12803=CARTESIAN_POINT('',(-2.85857864376269,-28.7414213562373,66.6));
#12804=CARTESIAN_POINT('',(-2.85857864376269,-28.7414213562373,40.5375));
#12805=CARTESIAN_POINT('',(-3.,-28.4,66.6));
#12806=CARTESIAN_POINT('',(-3.,-28.4,40.5375));
#12807=CARTESIAN_POINT('Origin',(-3.,0.,46.55));
#12808=CARTESIAN_POINT('',(-3.,24.4147650044641,69.9));
#12809=CARTESIAN_POINT('',(-3.,-7.275,69.9));
#12810=CARTESIAN_POINT('Origin',(-3.,25.,66.5));
#12811=CARTESIAN_POINT('',(-3.,7.275,23.2));
#12812=CARTESIAN_POINT('',(-3.,3.82537491619587,24.5060028672218));
#12813=CARTESIAN_POINT('Ctrl Pts',(-3.,4.25320571288467,23.2585265278816));
#12814=CARTESIAN_POINT('Ctrl Pts',(-3.,4.25320571288467,24.0552522778511));
#12815=CARTESIAN_POINT('Ctrl Pts',(-3.,3.82537491619587,24.5060028672218));
#12816=CARTESIAN_POINT('',(-3.,2.72087290883064,24.9567531585693));
#12817=CARTESIAN_POINT('Ctrl Pts',(-3.,3.82537491619587,24.5060028672218));
#12818=CARTESIAN_POINT('Ctrl Pts',(-3.,3.39754410088063,24.9567531585693));
#12819=CARTESIAN_POINT('Ctrl Pts',(-3.,2.72087290883064,24.9567531585693));
#12820=CARTESIAN_POINT('',(-3.,1.92196443676949,24.7450204730034));
#12821=CARTESIAN_POINT('Ctrl Pts',(-3.,2.72087290883064,24.9567531585693));
#12822=CARTESIAN_POINT('Ctrl Pts',(-3.,2.27776229381562,24.9567531585693));
#12823=CARTESIAN_POINT('Ctrl Pts',(-3.,1.92196443676949,24.7450204730034));
#12824=CARTESIAN_POINT('',(-3.,1.37953594326973,24.1545701563358));
#12825=CARTESIAN_POINT('Ctrl Pts',(-3.,1.92196443676949,24.7450204730034));
#12826=CARTESIAN_POINT('Ctrl Pts',(-3.,1.56616643071175,24.5332877874374));
#12827=CARTESIAN_POINT('Ctrl Pts',(-3.,1.37953594326973,24.1545701563358));
#12828=CARTESIAN_POINT('',(-3.,1.19290575385094,23.2956342935562));
#12829=CARTESIAN_POINT('Ctrl Pts',(-3.,1.37953594326973,24.1545701563358));
#12830=CARTESIAN_POINT('Ctrl Pts',(-3.,1.19290575385094,23.7758526742458));
#12831=CARTESIAN_POINT('Ctrl Pts',(-3.,1.19290575385094,23.2956342935562));
#12832=CARTESIAN_POINT('Ctrl Pts',(-3.,1.19290575385094,23.2956342935562));
#12833=CARTESIAN_POINT('Ctrl Pts',(-3.,1.19290575385094,23.1427574352851));
#12834=CARTESIAN_POINT('Ctrl Pts',(-3.,1.21228337796395,23.));
#12835=CARTESIAN_POINT('',(-3.,0.625375136733055,24.9));
#12836=CARTESIAN_POINT('',(-3.,0.625375136733055,34.1250000357628));
#12837=CARTESIAN_POINT('',(-3.,-1.5334241092205,24.9));
#12838=CARTESIAN_POINT('',(-3.,0.312687568366528,24.9));
#12839=CARTESIAN_POINT('',(-3.,-1.5334241092205,24.5223738789558));
#12840=CARTESIAN_POINT('',(-3.,-1.5334241092205,35.725));
#12841=CARTESIAN_POINT('',(-3.,0.201909989118576,24.5223738789558));
#12842=CARTESIAN_POINT('',(-3.,-0.766712054610252,24.5223738789558));
#12843=CARTESIAN_POINT('',(-3.,0.201909989118576,23.5313779652119));
#12844=CARTESIAN_POINT('',(-3.,0.201909989118576,35.5361869394779));
#12845=CARTESIAN_POINT('',(-3.,-1.29986360669136,23.5313779652119));
#12846=CARTESIAN_POINT('',(-3.,0.100954994559288,23.5313779652119));
#12847=CARTESIAN_POINT('',(-3.,-1.29986360669136,23.2));
#12848=CARTESIAN_POINT('',(-3.,-1.29986360669136,35.0406889826059));
#12849=CARTESIAN_POINT('',(-3.,-2.10532046854496,23.2));
#12850=CARTESIAN_POINT('',(-3.,7.275,23.2));
#12851=CARTESIAN_POINT('',(-3.,-2.10532046854496,24.9));
#12852=CARTESIAN_POINT('',(-3.,-2.10532046854496,34.1250000357628));
#12853=CARTESIAN_POINT('',(-3.,-4.26411971449852,24.9));
#12854=CARTESIAN_POINT('',(-3.,-1.05266023427248,24.9));
#12855=CARTESIAN_POINT('',(-3.,-4.26411971449852,24.5223738789558));
#12856=CARTESIAN_POINT('',(-3.,-4.26411971449852,35.725));
#12857=CARTESIAN_POINT('',(-3.,-2.52878561615944,24.5223738789558));
#12858=CARTESIAN_POINT('',(-3.,-2.13205985724926,24.5223738789558));
#12859=CARTESIAN_POINT('',(-3.,-2.52878561615944,23.5313779652119));
#12860=CARTESIAN_POINT('',(-3.,-2.52878561615944,35.5361869394779));
#12861=CARTESIAN_POINT('',(-3.,-4.03055921196938,23.5313779652119));
#12862=CARTESIAN_POINT('',(-3.,-1.26439280807972,23.5313779652119));
#12863=CARTESIAN_POINT('',(-3.,-4.03055921196938,35.0406889826059));
#12864=CARTESIAN_POINT('',(-3.,-4.03055921196938,65.1537516951561));
#12865=CARTESIAN_POINT('',(-3.,-2.52878561615944,65.1537516951561));
#12866=CARTESIAN_POINT('',(-3.,-2.01527960598469,65.1537516951561));
#12867=CARTESIAN_POINT('',(-3.,-2.52878561615944,63.7000000715256));
#12868=CARTESIAN_POINT('',(-3.,-2.52878561615944,55.851875847578));
#12869=CARTESIAN_POINT('',(-3.,-2.10532046854496,63.7000000715256));
#12870=CARTESIAN_POINT('',(-3.,-1.26439280807972,63.7000000715256));
#12871=CARTESIAN_POINT('',(-3.,-2.10532046854496,66.9));
#12872=CARTESIAN_POINT('',(-3.,-2.10532046854496,55.1250000357628));
#12873=CARTESIAN_POINT('',(-3.,-4.26411971449852,66.9));
#12874=CARTESIAN_POINT('',(-3.,-1.05266023427248,66.9));
#12875=CARTESIAN_POINT('',(-3.,-4.26411971449852,66.5223738789558));
#12876=CARTESIAN_POINT('',(-3.,-4.26411971449852,56.725));
#12877=CARTESIAN_POINT('',(-3.,-2.52878561615944,66.5223738789558));
#12878=CARTESIAN_POINT('',(-3.,-2.13205985724926,66.5223738789558));
#12879=CARTESIAN_POINT('',(-3.,-2.52878561615944,65.5313779652119));
#12880=CARTESIAN_POINT('',(-3.,-2.52878561615944,56.5361869394779));
#12881=CARTESIAN_POINT('',(-3.,-4.03055921196938,65.5313779652119));
#12882=CARTESIAN_POINT('',(-3.,-1.26439280807972,65.5313779652119));
#12883=CARTESIAN_POINT('',(-3.,-4.03055921196938,56.0406889826059));
#12884=CARTESIAN_POINT('',(-3.,-1.29986360669136,65.1537516951561));
#12885=CARTESIAN_POINT('',(-3.,0.201909989118576,65.1537516951561));
#12886=CARTESIAN_POINT('',(-3.,-0.64993180334568,65.1537516951561));
#12887=CARTESIAN_POINT('',(-3.,0.201909989118576,63.7000000715256));
#12888=CARTESIAN_POINT('',(-3.,0.201909989118576,55.851875847578));
#12889=CARTESIAN_POINT('',(-3.,0.625375136733055,63.7000000715256));
#12890=CARTESIAN_POINT('',(-3.,0.100954994559288,63.7000000715256));
#12891=CARTESIAN_POINT('',(-3.,0.625375136733055,66.9));
#12892=CARTESIAN_POINT('',(-3.,0.625375136733055,55.1250000357628));
#12893=CARTESIAN_POINT('',(-3.,-1.5334241092205,66.9));
#12894=CARTESIAN_POINT('',(-3.,0.312687568366528,66.9));
#12895=CARTESIAN_POINT('',(-3.,-1.5334241092205,66.5223738789558));
#12896=CARTESIAN_POINT('',(-3.,-1.5334241092205,56.725));
#12897=CARTESIAN_POINT('',(-3.,0.201909989118576,66.5223738789558));
#12898=CARTESIAN_POINT('',(-3.,-0.766712054610252,66.5223738789558));
#12899=CARTESIAN_POINT('',(-3.,0.201909989118576,65.5313779652119));
#12900=CARTESIAN_POINT('',(-3.,0.201909989118576,56.5361869394779));
#12901=CARTESIAN_POINT('',(-3.,-1.29986360669136,65.5313779652119));
#12902=CARTESIAN_POINT('',(-3.,0.100954994559288,65.5313779652119));
#12903=CARTESIAN_POINT('',(-3.,-1.29986360669136,56.0406889826059));
#12904=CARTESIAN_POINT('',(-3.,2.72305563092232,63.6454299330711));
#12905=CARTESIAN_POINT('',(-3.,3.53069551289082,63.8637107849121));
#12906=CARTESIAN_POINT('Ctrl Pts',(-3.,2.72305563092232,63.6454299330711));
#12907=CARTESIAN_POINT('Ctrl Pts',(-3.,3.17489743232727,63.6454299330711));
#12908=CARTESIAN_POINT('Ctrl Pts',(-3.,3.53069551289082,63.8637107849121));
#12909=CARTESIAN_POINT('',(-3.,4.06984962522984,64.4596180558205));
#12910=CARTESIAN_POINT('Ctrl Pts',(-3.,3.53069551289082,63.8637107849121));
#12911=CARTESIAN_POINT('Ctrl Pts',(-3.,3.88649359345436,64.0819919347763));
#12912=CARTESIAN_POINT('Ctrl Pts',(-3.,4.06984962522984,64.4596180558205));
#12913=CARTESIAN_POINT('',(-3.,4.25320571288467,65.2585265278816));
#12914=CARTESIAN_POINT('Ctrl Pts',(-3.,4.06984962522984,64.4596180558205));
#12915=CARTESIAN_POINT('Ctrl Pts',(-3.,4.25320571288467,64.8372441768646));
#12916=CARTESIAN_POINT('Ctrl Pts',(-3.,4.25320571288467,65.2585265278816));
#12917=CARTESIAN_POINT('',(-3.,3.82537491619587,66.5060028672218));
#12918=CARTESIAN_POINT('Ctrl Pts',(-3.,4.25320571288467,65.2585265278816));
#12919=CARTESIAN_POINT('Ctrl Pts',(-3.,4.25320571288467,66.0552522778511));
#12920=CARTESIAN_POINT('Ctrl Pts',(-3.,3.82537491619587,66.5060028672218));
#12921=CARTESIAN_POINT('',(-3.,2.72087290883064,66.9567531585693));
#12922=CARTESIAN_POINT('Ctrl Pts',(-3.,3.82537491619587,66.5060028672218));
#12923=CARTESIAN_POINT('Ctrl Pts',(-3.,3.39754410088063,66.9567531585693));
#12924=CARTESIAN_POINT('Ctrl Pts',(-3.,2.72087290883064,66.9567531585693));
#12925=CARTESIAN_POINT('',(-3.,1.92196443676949,66.7450204730034));
#12926=CARTESIAN_POINT('Ctrl Pts',(-3.,2.72087290883064,66.9567531585693));
#12927=CARTESIAN_POINT('Ctrl Pts',(-3.,2.27776229381562,66.9567531585693));
#12928=CARTESIAN_POINT('Ctrl Pts',(-3.,1.92196443676949,66.7450204730034));
#12929=CARTESIAN_POINT('',(-3.,1.37953594326973,66.1545701563358));
#12930=CARTESIAN_POINT('Ctrl Pts',(-3.,1.92196443676949,66.7450204730034));
#12931=CARTESIAN_POINT('Ctrl Pts',(-3.,1.56616643071175,66.5332877874374));
#12932=CARTESIAN_POINT('Ctrl Pts',(-3.,1.37953594326973,66.1545701563358));
#12933=CARTESIAN_POINT('',(-3.,1.19290575385094,65.2956342935562));
#12934=CARTESIAN_POINT('Ctrl Pts',(-3.,1.37953594326973,66.1545701563358));
#12935=CARTESIAN_POINT('Ctrl Pts',(-3.,1.19290575385094,65.7758526742458));
#12936=CARTESIAN_POINT('Ctrl Pts',(-3.,1.19290575385094,65.2956342935562));
#12937=CARTESIAN_POINT('',(-3.,1.38935878872872,64.4246930122376));
#12938=CARTESIAN_POINT('Ctrl Pts',(-3.,1.19290575385094,65.2956342935562));
#12939=CARTESIAN_POINT('Ctrl Pts',(-3.,1.19290575385094,64.80886759758));
#12940=CARTESIAN_POINT('Ctrl Pts',(-3.,1.38935878872872,64.4246930122376));
#12941=CARTESIAN_POINT('',(-3.,1.94597527384758,63.8429740309715));
#12942=CARTESIAN_POINT('Ctrl Pts',(-3.,1.38935878872872,64.4246930122376));
#12943=CARTESIAN_POINT('Ctrl Pts',(-3.,1.58581152558327,64.0405184268951));
#12944=CARTESIAN_POINT('Ctrl Pts',(-3.,1.94597527384758,63.8429740309715));
#12945=CARTESIAN_POINT('Ctrl Pts',(-3.,1.94597527384758,63.8429740309715));
#12946=CARTESIAN_POINT('Ctrl Pts',(-3.,2.30613887310028,63.6454299330711));
#12947=CARTESIAN_POINT('Ctrl Pts',(-3.,2.72305563092232,63.6454299330711));
#12948=CARTESIAN_POINT('',(-3.,-22.6896318495274,41.4999999403954));
#12949=CARTESIAN_POINT('',(-3.,-20.5886767506599,44.6432467103004));
#12950=CARTESIAN_POINT('',(-3.,-18.0197882014912,48.4865704628042));
#12951=CARTESIAN_POINT('',(-3.,-20.5886767506599,41.4999999403954));
#12952=CARTESIAN_POINT('',(-3.,-20.5886767506599,45.5966233551502));
#12953=CARTESIAN_POINT('',(-3.,-20.0811733752489,41.4999999403954));
#12954=CARTESIAN_POINT('',(-3.,-10.29433837533,41.4999999403953));
#12955=CARTESIAN_POINT('',(-3.,-20.0811733752489,45.5));
#12956=CARTESIAN_POINT('',(-3.,-20.0811733752489,44.0249999701977));
#12957=CARTESIAN_POINT('',(-3.,-20.6241474747658,45.5));
#12958=CARTESIAN_POINT('',(-3.,-10.0405866876245,45.5));
#12959=CARTESIAN_POINT('',(-3.,-22.7251025736332,42.3594816327095));
#12960=CARTESIAN_POINT('',(-3.,-17.1933097703598,50.6284336498615));
#12961=CARTESIAN_POINT('',(-3.,-22.7251025736332,45.5));
#12962=CARTESIAN_POINT('',(-3.,-22.7251025736332,44.4547408163547));
#12963=CARTESIAN_POINT('',(-3.,-23.2326057255268,45.5));
#12964=CARTESIAN_POINT('',(-3.,-11.3625512868166,45.5));
#12965=CARTESIAN_POINT('',(-3.,-23.2326057255268,41.4999999403954));
#12966=CARTESIAN_POINT('',(-3.,-23.2326057255268,46.025));
#12967=CARTESIAN_POINT('',(-3.,-11.6163028627634,41.4999999403953));
#12968=CARTESIAN_POINT('',(-3.,-17.4918144643307,41.4317871928215));
#12969=CARTESIAN_POINT('',(-3.,-16.4822646677494,41.7046384811401));
#12970=CARTESIAN_POINT('Ctrl Pts',(-3.,-17.4918144643307,41.4317871928215));
#12971=CARTESIAN_POINT('Ctrl Pts',(-3.,-16.9270123243332,41.4317871928215));
#12972=CARTESIAN_POINT('Ctrl Pts',(-3.,-16.4822646677494,41.7046384811401));
#12973=CARTESIAN_POINT('',(-3.,-15.8083220273256,42.4495224952698));
#12974=CARTESIAN_POINT('Ctrl Pts',(-3.,-16.4822646677494,41.7046384811401));
#12975=CARTESIAN_POINT('Ctrl Pts',(-3.,-16.0375170856714,41.9774897694588));
#12976=CARTESIAN_POINT('Ctrl Pts',(-3.,-15.8083220273256,42.4495224952698));
#12977=CARTESIAN_POINT('',(-3.,-15.5791269317269,43.4481580853462));
#12978=CARTESIAN_POINT('Ctrl Pts',(-3.,-15.8083220273256,42.4495224952698));
#12979=CARTESIAN_POINT('Ctrl Pts',(-3.,-15.5791269317269,42.9215552210808));
#12980=CARTESIAN_POINT('Ctrl Pts',(-3.,-15.5791269317269,43.4481580853462));
#12981=CARTESIAN_POINT('',(-3.,-16.1139154136181,45.0075035095215));
#12982=CARTESIAN_POINT('Ctrl Pts',(-3.,-15.5791269317269,43.4481580853462));
#12983=CARTESIAN_POINT('Ctrl Pts',(-3.,-15.5791269317269,44.4440655708313));
#12984=CARTESIAN_POINT('Ctrl Pts',(-3.,-16.1139154136181,45.0075035095215));
#12985=CARTESIAN_POINT('',(-3.,-17.4945430159569,45.5709411501884));
#12986=CARTESIAN_POINT('Ctrl Pts',(-3.,-16.1139154136181,45.0075035095215));
#12987=CARTESIAN_POINT('Ctrl Pts',(-3.,-16.6487039327621,45.5709411501884));
#12988=CARTESIAN_POINT('Ctrl Pts',(-3.,-17.4945430159569,45.5709411501884));
#12989=CARTESIAN_POINT('',(-3.,-18.4931787550449,45.30627566576));
#12990=CARTESIAN_POINT('Ctrl Pts',(-3.,-17.4945430159569,45.5709411501884));
#12991=CARTESIAN_POINT('Ctrl Pts',(-3.,-18.0484312474728,45.5709411501884));
#12992=CARTESIAN_POINT('Ctrl Pts',(-3.,-18.4931787550449,45.30627566576));
#12993=CARTESIAN_POINT('',(-3.,-19.1712143719196,44.5682128071785));
#12994=CARTESIAN_POINT('Ctrl Pts',(-3.,-18.4931787550449,45.30627566576));
#12995=CARTESIAN_POINT('Ctrl Pts',(-3.,-18.9379265606403,45.0416098833084));
#12996=CARTESIAN_POINT('Ctrl Pts',(-3.,-19.1712143719196,44.5682128071785));
#12997=CARTESIAN_POINT('',(-3.,-19.4045021831989,43.4945430159569));
#12998=CARTESIAN_POINT('Ctrl Pts',(-3.,-19.1712143719196,44.5682128071785));
#12999=CARTESIAN_POINT('Ctrl Pts',(-3.,-19.4045021831989,44.0948157310486));
#13000=CARTESIAN_POINT('Ctrl Pts',(-3.,-19.4045021831989,43.4945430159569));
#13001=CARTESIAN_POINT('',(-3.,-19.1589361131191,42.4058662652969));
#13002=CARTESIAN_POINT('Ctrl Pts',(-3.,-19.4045021831989,43.4945430159569));
#13003=CARTESIAN_POINT('Ctrl Pts',(-3.,-19.4045021831989,42.8860844969749));
#13004=CARTESIAN_POINT('Ctrl Pts',(-3.,-19.1589361131191,42.4058662652969));
#13005=CARTESIAN_POINT('',(-3.,-18.4631651341915,41.6787176132202));
#13006=CARTESIAN_POINT('Ctrl Pts',(-3.,-19.1589361131191,42.4058662652969));
#13007=CARTESIAN_POINT('Ctrl Pts',(-3.,-18.9133697450161,41.9256480336189));
#13008=CARTESIAN_POINT('Ctrl Pts',(-3.,-18.4631651341915,41.6787176132202));
#13009=CARTESIAN_POINT('Ctrl Pts',(-3.,-18.4631651341915,41.6787176132202));
#13010=CARTESIAN_POINT('Ctrl Pts',(-3.,-18.0129605233669,41.4317871928215));
#13011=CARTESIAN_POINT('Ctrl Pts',(-3.,-17.4918144643307,41.4317871928215));
#13012=CARTESIAN_POINT('',(-3.,-7.9602041944578E-16,54.));
#13013=CARTESIAN_POINT('Origin',(-3.,0.,47.5));
#13014=CARTESIAN_POINT('',(-3.,21.5081855356693,41.4317871928215));
#13015=CARTESIAN_POINT('',(-3.,22.5177353322506,41.7046384811401));
#13016=CARTESIAN_POINT('Ctrl Pts',(-3.,21.5081855356693,41.4317871928215));
#13017=CARTESIAN_POINT('Ctrl Pts',(-3.,22.0729876756668,41.4317871928215));
#13018=CARTESIAN_POINT('Ctrl Pts',(-3.,22.5177353322506,41.7046384811401));
#13019=CARTESIAN_POINT('',(-3.,23.1916779726744,42.4495224952698));
#13020=CARTESIAN_POINT('Ctrl Pts',(-3.,22.5177353322506,41.7046384811401));
#13021=CARTESIAN_POINT('Ctrl Pts',(-3.,22.9624829143286,41.9774897694588));
#13022=CARTESIAN_POINT('Ctrl Pts',(-3.,23.1916779726744,42.4495224952698));
#13023=CARTESIAN_POINT('',(-3.,23.4208730682731,43.4481580853462));
#13024=CARTESIAN_POINT('Ctrl Pts',(-3.,23.1916779726744,42.4495224952698));
#13025=CARTESIAN_POINT('Ctrl Pts',(-3.,23.4208730682731,42.9215552210808));
#13026=CARTESIAN_POINT('Ctrl Pts',(-3.,23.4208730682731,43.4481580853462));
#13027=CARTESIAN_POINT('',(-3.,22.8860845863819,45.0075035095215));
#13028=CARTESIAN_POINT('Ctrl Pts',(-3.,23.4208730682731,43.4481580853462));
#13029=CARTESIAN_POINT('Ctrl Pts',(-3.,23.4208730682731,44.4440655708313));
#13030=CARTESIAN_POINT('Ctrl Pts',(-3.,22.8860845863819,45.0075035095215));
#13031=CARTESIAN_POINT('',(-3.,21.5054569840431,45.5709411501884));
#13032=CARTESIAN_POINT('Ctrl Pts',(-3.,22.8860845863819,45.0075035095215));
#13033=CARTESIAN_POINT('Ctrl Pts',(-3.,22.3512960672379,45.5709411501884));
#13034=CARTESIAN_POINT('Ctrl Pts',(-3.,21.5054569840431,45.5709411501884));
#13035=CARTESIAN_POINT('',(-3.,20.5068212449551,45.30627566576));
#13036=CARTESIAN_POINT('Ctrl Pts',(-3.,21.5054569840431,45.5709411501884));
#13037=CARTESIAN_POINT('Ctrl Pts',(-3.,20.9515687525272,45.5709411501884));
#13038=CARTESIAN_POINT('Ctrl Pts',(-3.,20.5068212449551,45.30627566576));
#13039=CARTESIAN_POINT('',(-3.,19.8287856280804,44.5682128071785));
#13040=CARTESIAN_POINT('Ctrl Pts',(-3.,20.5068212449551,45.30627566576));
#13041=CARTESIAN_POINT('Ctrl Pts',(-3.,20.0620734393597,45.0416098833084));
#13042=CARTESIAN_POINT('Ctrl Pts',(-3.,19.8287856280804,44.5682128071785));
#13043=CARTESIAN_POINT('',(-3.,19.5954978168011,43.4945430159569));
#13044=CARTESIAN_POINT('Ctrl Pts',(-3.,19.8287856280804,44.5682128071785));
#13045=CARTESIAN_POINT('Ctrl Pts',(-3.,19.5954978168011,44.0948157310486));
#13046=CARTESIAN_POINT('Ctrl Pts',(-3.,19.5954978168011,43.4945430159569));
#13047=CARTESIAN_POINT('',(-3.,19.8410638868809,42.4058662652969));
#13048=CARTESIAN_POINT('Ctrl Pts',(-3.,19.5954978168011,43.4945430159569));
#13049=CARTESIAN_POINT('Ctrl Pts',(-3.,19.5954978168011,42.8860844969749));
#13050=CARTESIAN_POINT('Ctrl Pts',(-3.,19.8410638868809,42.4058662652969));
#13051=CARTESIAN_POINT('',(-3.,20.5368348658085,41.6787176132202));
#13052=CARTESIAN_POINT('Ctrl Pts',(-3.,19.8410638868809,42.4058662652969));
#13053=CARTESIAN_POINT('Ctrl Pts',(-3.,20.0866302549839,41.9256480336189));
#13054=CARTESIAN_POINT('Ctrl Pts',(-3.,20.5368348658085,41.6787176132202));
#13055=CARTESIAN_POINT('Ctrl Pts',(-3.,20.5368348658085,41.6787176132202));
#13056=CARTESIAN_POINT('Ctrl Pts',(-3.,20.9870394766331,41.4317871928215));
#13057=CARTESIAN_POINT('Ctrl Pts',(-3.,21.5081855356693,41.4317871928215));
#13058=CARTESIAN_POINT('',(-3.,16.3103681504726,41.4999999403954));
#13059=CARTESIAN_POINT('',(-3.,18.4113232493401,44.6432467103004));
#13060=CARTESIAN_POINT('',(-3.,14.9585828206595,39.4775888599155));
#13061=CARTESIAN_POINT('',(-3.,18.4113232493401,41.4999999403954));
#13062=CARTESIAN_POINT('',(-3.,18.4113232493401,45.5966233551502));
#13063=CARTESIAN_POINT('',(-3.,18.9188266247511,41.4999999403954));
#13064=CARTESIAN_POINT('',(-3.,9.20566162467003,41.4999999403953));
#13065=CARTESIAN_POINT('',(-3.,18.9188266247511,45.5));
#13066=CARTESIAN_POINT('',(-3.,18.9188266247511,44.0249999701977));
#13067=CARTESIAN_POINT('',(-3.,18.3758525252342,45.5));
#13068=CARTESIAN_POINT('',(-3.,9.45941331237555,45.5));
#13069=CARTESIAN_POINT('',(-3.,16.2748974263668,42.3594816327095));
#13070=CARTESIAN_POINT('',(-3.,15.777830067132,41.6164628160299));
#13071=CARTESIAN_POINT('',(-3.,16.2748974263668,45.5));
#13072=CARTESIAN_POINT('',(-3.,16.2748974263668,44.4547408163547));
#13073=CARTESIAN_POINT('',(-3.,15.7673942744732,45.5));
#13074=CARTESIAN_POINT('',(-3.,8.1374487131834,45.5));
#13075=CARTESIAN_POINT('',(-3.,15.7673942744732,41.4999999403954));
#13076=CARTESIAN_POINT('',(-3.,15.7673942744732,46.025));
#13077=CARTESIAN_POINT('',(-3.,7.8836971372366,41.4999999403953));
#13078=CARTESIAN_POINT('Origin',(-2.225,-25.,66.5));
#13079=CARTESIAN_POINT('',(-1.45,-25.,68.2));
#13080=CARTESIAN_POINT('',(-2.225,-25.,68.975));
#13081=CARTESIAN_POINT('Origin',(-1.45,-25.,66.5));
#13082=CARTESIAN_POINT('Origin',(-2.92928932188134,25.,66.5));
#13083=CARTESIAN_POINT('',(-2.85857864376269,25.,69.6085786437627));
#13084=CARTESIAN_POINT('Origin',(-2.85857864376269,25.,66.5));
#13085=CARTESIAN_POINT('',(-2.9896446609407,25.,69.9249999999999));
#13086=CARTESIAN_POINT('',(-2.92928932188134,25.,69.7792893218814));
#13087=CARTESIAN_POINT('',(-2.98994700660664,25.1,69.9242700729927));
#13088=CARTESIAN_POINT('Ctrl Pts',(-2.9896446609407,25.,69.9249999999999));
#13089=CARTESIAN_POINT('Ctrl Pts',(-2.98964466094069,25.0500000000001,69.925));
#13090=CARTESIAN_POINT('Ctrl Pts',(-2.98994700660664,25.1,69.9242700729927));
#13091=CARTESIAN_POINT('Ctrl Pts',(-2.98994700660664,25.1,69.9242700729927));
#13092=CARTESIAN_POINT('Ctrl Pts',(-2.99238240184869,25.5027501492823,69.9183905087696));
#13093=CARTESIAN_POINT('Ctrl Pts',(-2.99447851800497,25.9263094322197,69.8364130892601));
#13094=CARTESIAN_POINT('Ctrl Pts',(-2.99745891948881,26.7431214573392,69.5052855480682));
#13095=CARTESIAN_POINT('Ctrl Pts',(-2.99822330470336,27.1309143229168,69.2420564500924));
#13096=CARTESIAN_POINT('Ctrl Pts',(-2.99822330470336,27.7420564500924,68.6309143229168));
#13097=CARTESIAN_POINT('Ctrl Pts',(-2.99745891948881,28.0052855480682,68.2431214573392));
#13098=CARTESIAN_POINT('Ctrl Pts',(-2.99447851800497,28.3364130892601,67.4263094322197));
#13099=CARTESIAN_POINT('Ctrl Pts',(-2.99238240184869,28.4183905087696,67.0027501492822));
#13100=CARTESIAN_POINT('Ctrl Pts',(-2.98994700660664,28.4242700729927,66.6));
#13101=CARTESIAN_POINT('Ctrl Pts',(-3.,24.4147650044641,69.9));
#13102=CARTESIAN_POINT('Ctrl Pts',(-2.98964466094078,24.7073825022338,69.9249999999997));
#13103=CARTESIAN_POINT('Ctrl Pts',(-2.9896446609407,25.,69.9249999999999));
#13104=CARTESIAN_POINT('Origin',(-2.225,25.,66.5));
#13105=CARTESIAN_POINT('',(-1.45,25.,68.2));
#13106=CARTESIAN_POINT('',(-2.225,25.,68.975));
#13107=CARTESIAN_POINT('Origin',(-1.45,25.,66.5));
#13108=CARTESIAN_POINT('Origin',(-2.92928932188134,7.275,23.0292893218813));
#13109=CARTESIAN_POINT('',(-2.69947963063977,-2.10532046854496,22.4744796485212));
#13110=CARTESIAN_POINT('',(-2.98084332489689,-1.29986360669136,23.1537516951561));
#13111=CARTESIAN_POINT('',(-3.02322456252495,-1.29986360669136,23.2560690538279));
#13112=CARTESIAN_POINT('',(-2.98084332489689,0.201909989118576,23.1537516951561));
#13113=CARTESIAN_POINT('',(-2.98084332489689,2.98756819665432,23.1537516951561));
#13114=CARTESIAN_POINT('',(-2.9564690384473,0.201909989118577,23.0949069622363));
#13115=CARTESIAN_POINT('Origin',(-3.,0.201909989118576,23.1537516951561));
#13116=CARTESIAN_POINT('',(-2.75,0.201909989118576,23.1537516951561));
#13117=CARTESIAN_POINT('',(-3.,0.201909989118576,23.1537516951561));
#13118=CARTESIAN_POINT('',(-2.75,0.201909989118576,23.1537516951561));
#13119=CARTESIAN_POINT('Origin',(-3.,-1.29986360669136,23.1537516951561));
#13120=CARTESIAN_POINT('',(-2.75,-1.29986360669136,23.1537516951561));
#13121=CARTESIAN_POINT('',(-3.,-1.29986360669136,23.1537516951561));
#13122=CARTESIAN_POINT('',(-2.75,-1.29986360669136,23.1537516951561));
#13123=CARTESIAN_POINT('Origin',(-2.92928932188134,7.275,23.0292893218813));
#13124=CARTESIAN_POINT('Origin',(-2.92928932188134,25.1,66.6));
#13125=CARTESIAN_POINT('',(-3.,25.1,69.9));
#13126=CARTESIAN_POINT('Origin',(-2.92928932188135,-7.275,70.0707106781187));
#13127=CARTESIAN_POINT('',(-2.85857864376268,-25.1,70.2414213562373));
#13128=CARTESIAN_POINT('',(-3.,-25.1,69.9));
#13129=CARTESIAN_POINT('',(-2.85857864376269,-7.275,70.2414213562373));
#13130=CARTESIAN_POINT('Origin',(-2.92928932188135,-25.1,66.6));
#13131=CARTESIAN_POINT('Origin',(-2.85857864376269,-25.1,66.6));
#13132=CARTESIAN_POINT('Origin',(-2.75,-14.55,70.35));
#13133=CARTESIAN_POINT('',(-2.5,-25.1,70.6));
#13134=CARTESIAN_POINT('Origin',(-2.75,-25.1,66.6));
#13135=CARTESIAN_POINT('',(-3.,-28.6,66.6));
#13136=CARTESIAN_POINT('Origin',(-2.75,-28.85,34.525));
#13137=CARTESIAN_POINT('',(-3.,-28.6,26.5));
#13138=CARTESIAN_POINT('Origin',(-2.75,-25.1,26.5));
#13139=CARTESIAN_POINT('Origin',(-3.,-2.52878561615944,23.1537516951561));
#13140=CARTESIAN_POINT('',(-2.75,-2.52878561615944,23.1537516951561));
#13141=CARTESIAN_POINT('',(-3.,-2.52878561615944,23.1537516951561));
#13142=CARTESIAN_POINT('',(-2.75,-2.52878561615944,23.1537516951561));
#13143=CARTESIAN_POINT('Origin',(-3.,-4.03055921196938,23.1537516951561));
#13144=CARTESIAN_POINT('',(-2.75,-4.03055921196938,23.1537516951561));
#13145=CARTESIAN_POINT('',(-3.,-4.03055921196938,23.1537516951561));
#13146=CARTESIAN_POINT('',(-2.75,-4.03055921196938,23.1537516951561));
#13147=CARTESIAN_POINT('Origin',(-2.75,2.7230557333678,23.3010915458202));
#13148=CARTESIAN_POINT('',(-2.75,1.19290575385094,23.2956342935562));
#13149=CARTESIAN_POINT('Ctrl Pts',(-2.75,1.19290575385094,23.2956342935562));
#13150=CARTESIAN_POINT('Ctrl Pts',(-2.75,1.19290575385094,23.1158170345574));
#13151=CARTESIAN_POINT('Ctrl Pts',(-2.75,1.21971470205851,22.95));
#13152=CARTESIAN_POINT('',(-2.75,1.37953594326973,24.1545701563358));
#13153=CARTESIAN_POINT('Ctrl Pts',(-2.75,1.37953594326973,24.1545701563358));
#13154=CARTESIAN_POINT('Ctrl Pts',(-2.75,1.19290575385094,23.7758526742458));
#13155=CARTESIAN_POINT('Ctrl Pts',(-2.75,1.19290575385094,23.2956342935562));
#13156=CARTESIAN_POINT('',(-2.75,1.92196443676949,24.7450204730034));
#13157=CARTESIAN_POINT('Ctrl Pts',(-2.75,1.92196443676949,24.7450204730034));
#13158=CARTESIAN_POINT('Ctrl Pts',(-2.75,1.56616643071175,24.5332877874374));
#13159=CARTESIAN_POINT('Ctrl Pts',(-2.75,1.37953594326973,24.1545701563358));
#13160=CARTESIAN_POINT('',(-2.75,2.72087290883064,24.9567531585693));
#13161=CARTESIAN_POINT('Ctrl Pts',(-2.75,2.72087290883064,24.9567531585693));
#13162=CARTESIAN_POINT('Ctrl Pts',(-2.75,2.27776229381562,24.9567531585693));
#13163=CARTESIAN_POINT('Ctrl Pts',(-2.75,1.92196443676949,24.7450204730034));
#13164=CARTESIAN_POINT('',(-2.75,3.82537491619587,24.5060028672218));
#13165=CARTESIAN_POINT('Ctrl Pts',(-2.75,3.82537491619587,24.5060028672218));
#13166=CARTESIAN_POINT('Ctrl Pts',(-2.75,3.39754410088063,24.9567531585693));
#13167=CARTESIAN_POINT('Ctrl Pts',(-2.75,2.72087290883064,24.9567531585693));
#13168=CARTESIAN_POINT('Ctrl Pts',(-2.75,4.25320571288467,23.2585265278816));
#13169=CARTESIAN_POINT('Ctrl Pts',(-2.75,4.25320571288467,24.0552522778511));
#13170=CARTESIAN_POINT('Ctrl Pts',(-2.75,3.82537491619587,24.5060028672218));
#13171=CARTESIAN_POINT('Origin',(-3.,-4.03055921196938,23.5313779652119));
#13172=CARTESIAN_POINT('',(-2.75,-4.03055921196938,23.5313779652119));
#13173=CARTESIAN_POINT('',(-3.,-4.03055921196938,23.5313779652119));
#13174=CARTESIAN_POINT('',(-2.75,-4.03055921196938,23.5313779652119));
#13175=CARTESIAN_POINT('Origin',(-3.,-2.52878561615944,23.5313779652119));
#13176=CARTESIAN_POINT('',(-2.75,-2.52878561615944,23.5313779652119));
#13177=CARTESIAN_POINT('',(-3.,-2.52878561615944,23.5313779652119));
#13178=CARTESIAN_POINT('',(-2.75,-2.52878561615944,23.5313779652119));
#13179=CARTESIAN_POINT('Origin',(-3.,-2.52878561615944,24.5223738789558));
#13180=CARTESIAN_POINT('',(-2.75,-2.52878561615944,24.5223738789558));
#13181=CARTESIAN_POINT('',(-3.,-2.52878561615944,24.5223738789558));
#13182=CARTESIAN_POINT('',(-2.75,-2.52878561615944,24.5223738789558));
#13183=CARTESIAN_POINT('Origin',(-3.,-4.26411971449852,24.5223738789558));
#13184=CARTESIAN_POINT('',(-2.75,-4.26411971449852,24.5223738789558));
#13185=CARTESIAN_POINT('',(-3.,-4.26411971449852,24.5223738789558));
#13186=CARTESIAN_POINT('',(-2.75,-4.26411971449852,24.5223738789558));
#13187=CARTESIAN_POINT('Origin',(-3.,-4.26411971449852,24.9));
#13188=CARTESIAN_POINT('',(-2.75,-4.26411971449852,24.9));
#13189=CARTESIAN_POINT('',(-3.,-4.26411971449852,24.9));
#13190=CARTESIAN_POINT('',(-2.75,-4.26411971449852,24.9));
#13191=CARTESIAN_POINT('Origin',(-3.,-2.10532046854496,24.9));
#13192=CARTESIAN_POINT('',(-2.75,-2.10532046854496,24.9));
#13193=CARTESIAN_POINT('',(-3.,-2.10532046854496,24.9));
#13194=CARTESIAN_POINT('',(-2.75,-2.10532046854496,24.9));
#13195=CARTESIAN_POINT('Origin',(-3.,-2.10532046854496,21.7000000715256));
#13196=CARTESIAN_POINT('',(-2.75,-2.10532046854496,21.7000000715256));
#13197=CARTESIAN_POINT('Origin',(-2.75,-3.18472009152174,23.3000000357628));
#13198=CARTESIAN_POINT('Origin',(-3.,-1.29986360669136,23.5313779652119));
#13199=CARTESIAN_POINT('',(-2.75,-1.29986360669136,23.5313779652119));
#13200=CARTESIAN_POINT('',(-3.,-1.29986360669136,23.5313779652119));
#13201=CARTESIAN_POINT('',(-2.75,-1.29986360669136,23.5313779652119));
#13202=CARTESIAN_POINT('Origin',(-3.,0.201909989118576,23.5313779652119));
#13203=CARTESIAN_POINT('',(-2.75,0.201909989118576,23.5313779652119));
#13204=CARTESIAN_POINT('',(-3.,0.201909989118576,23.5313779652119));
#13205=CARTESIAN_POINT('',(-2.75,0.201909989118576,23.5313779652119));
#13206=CARTESIAN_POINT('Origin',(-3.,0.201909989118576,24.5223738789558));
#13207=CARTESIAN_POINT('',(-2.75,0.201909989118576,24.5223738789558));
#13208=CARTESIAN_POINT('',(-3.,0.201909989118576,24.5223738789558));
#13209=CARTESIAN_POINT('',(-2.75,0.201909989118576,24.5223738789558));
#13210=CARTESIAN_POINT('Origin',(-3.,-1.5334241092205,24.5223738789558));
#13211=CARTESIAN_POINT('',(-2.75,-1.5334241092205,24.5223738789558));
#13212=CARTESIAN_POINT('',(-3.,-1.5334241092205,24.5223738789558));
#13213=CARTESIAN_POINT('',(-2.75,-1.5334241092205,24.5223738789558));
#13214=CARTESIAN_POINT('Origin',(-3.,-1.5334241092205,24.9));
#13215=CARTESIAN_POINT('',(-2.75,-1.5334241092205,24.9));
#13216=CARTESIAN_POINT('',(-3.,-1.5334241092205,24.9));
#13217=CARTESIAN_POINT('',(-2.75,-1.5334241092205,24.9));
#13218=CARTESIAN_POINT('Origin',(-3.,0.625375136733055,24.9));
#13219=CARTESIAN_POINT('',(-2.75,0.625375136733055,24.9));
#13220=CARTESIAN_POINT('',(-3.,0.625375136733055,24.9));
#13221=CARTESIAN_POINT('',(-2.75,0.625375136733055,24.9));
#13222=CARTESIAN_POINT('Origin',(-3.,0.625375136733055,21.7000000715256));
#13223=CARTESIAN_POINT('',(-2.75,0.625375136733055,21.7000000715256));
#13224=CARTESIAN_POINT('Origin',(-2.75,-0.454024486243725,23.3000000357628));
#13225=CARTESIAN_POINT('Ctrl Pts',(-3.90882250993909,1.19290575385094,24.0392854381073));
#13226=CARTESIAN_POINT('Ctrl Pts',(-1.59117749006091,1.19290575385094,24.0392854381073));
#13227=CARTESIAN_POINT('Ctrl Pts',(-3.90882250993909,1.19290575385094,23.6674598658318));
#13228=CARTESIAN_POINT('Ctrl Pts',(-1.59117749006091,1.19290575385094,23.6674598658318));
#13229=CARTESIAN_POINT('Ctrl Pts',(-3.90882250993909,1.19290575385094,23.2956342935562));
#13230=CARTESIAN_POINT('Ctrl Pts',(-1.59117749006091,1.19290575385094,23.2956342935562));
#13231=CARTESIAN_POINT('Ctrl Pts',(-3.90882250993909,1.19290575385094,22.80886759758));
#13232=CARTESIAN_POINT('Ctrl Pts',(-1.59117749006091,1.19290575385094,22.80886759758));
#13233=CARTESIAN_POINT('Ctrl Pts',(-3.90882250993909,1.38935878872872,22.4246930122375));
#13234=CARTESIAN_POINT('Ctrl Pts',(-1.59117749006091,1.38935878872872,22.4246930122375));
#13235=CARTESIAN_POINT('Ctrl Pts',(-3.90882250993909,1.57799645627673,22.0558018024107));
#13236=CARTESIAN_POINT('Ctrl Pts',(-1.59117749006091,1.57799645627673,22.0558018024107));
#13237=CARTESIAN_POINT('Ctrl Pts',(-3.90882250993909,1.76663412382475,21.6869105925839));
#13238=CARTESIAN_POINT('Ctrl Pts',(-1.59117749006091,1.76663412382475,21.6869105925839));
#13239=CARTESIAN_POINT('',(-3.,1.19290575385094,23.2956342935562));
#13240=CARTESIAN_POINT('Ctrl Pts',(-3.,1.37953594326973,24.1545701563358));
#13241=CARTESIAN_POINT('Ctrl Pts',(-2.75,1.37953594326973,24.1545701563358));
#13242=CARTESIAN_POINT('Ctrl Pts',(-3.,1.19290575385094,23.7758526742458));
#13243=CARTESIAN_POINT('Ctrl Pts',(-2.75,1.19290575385094,23.7758526742458));
#13244=CARTESIAN_POINT('Ctrl Pts',(-3.,1.19290575385094,23.2956342935562));
#13245=CARTESIAN_POINT('Ctrl Pts',(-2.75,1.19290575385094,23.2956342935562));
#13246=CARTESIAN_POINT('',(-3.,1.37953594326973,24.1545701563358));
#13247=CARTESIAN_POINT('Ctrl Pts',(-3.,1.92196443676949,24.7450204730034));
#13248=CARTESIAN_POINT('Ctrl Pts',(-2.75,1.92196443676949,24.7450204730034));
#13249=CARTESIAN_POINT('Ctrl Pts',(-3.,1.56616643071175,24.5332877874374));
#13250=CARTESIAN_POINT('Ctrl Pts',(-2.75,1.56616643071175,24.5332877874374));
#13251=CARTESIAN_POINT('Ctrl Pts',(-3.,1.37953594326973,24.1545701563358));
#13252=CARTESIAN_POINT('Ctrl Pts',(-2.75,1.37953594326973,24.1545701563358));
#13253=CARTESIAN_POINT('',(-3.,1.92196443676949,24.7450204730034));
#13254=CARTESIAN_POINT('Ctrl Pts',(-3.,2.72087290883064,24.9567531585693));
#13255=CARTESIAN_POINT('Ctrl Pts',(-2.75,2.72087290883064,24.9567531585693));
#13256=CARTESIAN_POINT('Ctrl Pts',(-3.,2.27776229381562,24.9567531585693));
#13257=CARTESIAN_POINT('Ctrl Pts',(-2.75,2.27776229381562,24.9567531585693));
#13258=CARTESIAN_POINT('Ctrl Pts',(-3.,1.92196443676949,24.7450204730034));
#13259=CARTESIAN_POINT('Ctrl Pts',(-2.75,1.92196443676949,24.7450204730034));
#13260=CARTESIAN_POINT('',(-3.,2.72087290883064,24.9567531585693));
#13261=CARTESIAN_POINT('Ctrl Pts',(-3.,3.82537491619587,24.5060028672218));
#13262=CARTESIAN_POINT('Ctrl Pts',(-2.75,3.82537491619587,24.5060028672218));
#13263=CARTESIAN_POINT('Ctrl Pts',(-3.,3.39754410088063,24.9567531585693));
#13264=CARTESIAN_POINT('Ctrl Pts',(-2.75,3.39754410088063,24.9567531585693));
#13265=CARTESIAN_POINT('Ctrl Pts',(-3.,2.72087290883064,24.9567531585693));
#13266=CARTESIAN_POINT('Ctrl Pts',(-2.75,2.72087290883064,24.9567531585693));
#13267=CARTESIAN_POINT('',(-3.,3.82537491619587,24.5060028672218));
#13268=CARTESIAN_POINT('Ctrl Pts',(-3.,4.25320571288467,23.2585265278816));
#13269=CARTESIAN_POINT('Ctrl Pts',(-2.75,4.25320571288467,23.2585265278816));
#13270=CARTESIAN_POINT('Ctrl Pts',(-3.,4.25320571288467,24.0552522778511));
#13271=CARTESIAN_POINT('Ctrl Pts',(-2.75,4.25320571288467,24.0552522778511));
#13272=CARTESIAN_POINT('Ctrl Pts',(-3.,3.82537491619587,24.5060028672218));
#13273=CARTESIAN_POINT('Ctrl Pts',(-2.75,3.82537491619587,24.5060028672218));
#13274=CARTESIAN_POINT('Origin',(-3.,-4.03055921196938,65.1537516951561));
#13275=CARTESIAN_POINT('',(-2.75,-4.03055921196938,65.1537516951561));
#13276=CARTESIAN_POINT('',(-3.,-4.03055921196938,65.1537516951561));
#13277=CARTESIAN_POINT('',(-2.75,-2.52878561615944,65.1537516951561));
#13278=CARTESIAN_POINT('',(-2.75,-4.03055921196938,65.1537516951561));
#13279=CARTESIAN_POINT('',(-3.,-2.52878561615944,65.1537516951561));
#13280=CARTESIAN_POINT('Origin',(-3.,-4.03055921196938,65.5313779652119));
#13281=CARTESIAN_POINT('',(-2.75,-4.03055921196938,65.5313779652119));
#13282=CARTESIAN_POINT('',(-3.,-4.03055921196938,65.5313779652119));
#13283=CARTESIAN_POINT('',(-2.75,-4.03055921196938,65.5313779652119));
#13284=CARTESIAN_POINT('Origin',(-3.,-2.52878561615944,65.5313779652119));
#13285=CARTESIAN_POINT('',(-2.75,-2.52878561615944,65.5313779652119));
#13286=CARTESIAN_POINT('',(-3.,-2.52878561615944,65.5313779652119));
#13287=CARTESIAN_POINT('',(-2.75,-2.52878561615944,65.5313779652119));
#13288=CARTESIAN_POINT('Origin',(-3.,-2.52878561615944,66.5223738789558));
#13289=CARTESIAN_POINT('',(-2.75,-2.52878561615944,66.5223738789558));
#13290=CARTESIAN_POINT('',(-3.,-2.52878561615944,66.5223738789558));
#13291=CARTESIAN_POINT('',(-2.75,-2.52878561615944,66.5223738789558));
#13292=CARTESIAN_POINT('Origin',(-3.,-4.26411971449852,66.5223738789558));
#13293=CARTESIAN_POINT('',(-2.75,-4.26411971449852,66.5223738789558));
#13294=CARTESIAN_POINT('',(-3.,-4.26411971449852,66.5223738789558));
#13295=CARTESIAN_POINT('',(-2.75,-4.26411971449852,66.5223738789558));
#13296=CARTESIAN_POINT('Origin',(-3.,-4.26411971449852,66.9));
#13297=CARTESIAN_POINT('',(-2.75,-4.26411971449852,66.9));
#13298=CARTESIAN_POINT('',(-3.,-4.26411971449852,66.9));
#13299=CARTESIAN_POINT('',(-2.75,-4.26411971449852,66.9));
#13300=CARTESIAN_POINT('Origin',(-3.,-2.10532046854496,66.9));
#13301=CARTESIAN_POINT('',(-2.75,-2.10532046854496,66.9));
#13302=CARTESIAN_POINT('',(-3.,-2.10532046854496,66.9));
#13303=CARTESIAN_POINT('',(-2.75,-2.10532046854496,66.9));
#13304=CARTESIAN_POINT('Origin',(-3.,-2.10532046854496,63.7000000715256));
#13305=CARTESIAN_POINT('',(-2.75,-2.10532046854496,63.7000000715256));
#13306=CARTESIAN_POINT('',(-3.,-2.10532046854496,63.7000000715256));
#13307=CARTESIAN_POINT('',(-2.75,-2.10532046854496,63.7000000715256));
#13308=CARTESIAN_POINT('Origin',(-3.,-2.52878561615944,63.7000000715256));
#13309=CARTESIAN_POINT('',(-2.75,-2.52878561615944,63.7000000715256));
#13310=CARTESIAN_POINT('',(-3.,-2.52878561615944,63.7000000715256));
#13311=CARTESIAN_POINT('',(-2.75,-2.52878561615944,63.7000000715256));
#13312=CARTESIAN_POINT('Origin',(-3.,-2.52878561615944,65.1537516951561));
#13313=CARTESIAN_POINT('',(-2.75,-2.52878561615944,65.1537516951561));
#13314=CARTESIAN_POINT('Origin',(-2.75,-3.18472009152174,65.3000000357628));
#13315=CARTESIAN_POINT('Origin',(-3.,-1.29986360669136,65.1537516951561));
#13316=CARTESIAN_POINT('',(-2.75,-1.29986360669136,65.1537516951561));
#13317=CARTESIAN_POINT('',(-3.,-1.29986360669136,65.1537516951561));
#13318=CARTESIAN_POINT('',(-2.75,0.201909989118576,65.1537516951561));
#13319=CARTESIAN_POINT('',(-2.75,-1.29986360669136,65.1537516951561));
#13320=CARTESIAN_POINT('',(-3.,0.201909989118576,65.1537516951561));
#13321=CARTESIAN_POINT('Origin',(-3.,-1.29986360669136,65.5313779652119));
#13322=CARTESIAN_POINT('',(-2.75,-1.29986360669136,65.5313779652119));
#13323=CARTESIAN_POINT('',(-3.,-1.29986360669136,65.5313779652119));
#13324=CARTESIAN_POINT('',(-2.75,-1.29986360669136,65.5313779652119));
#13325=CARTESIAN_POINT('Origin',(-3.,0.201909989118576,65.5313779652119));
#13326=CARTESIAN_POINT('',(-2.75,0.201909989118576,65.5313779652119));
#13327=CARTESIAN_POINT('',(-3.,0.201909989118576,65.5313779652119));
#13328=CARTESIAN_POINT('',(-2.75,0.201909989118576,65.5313779652119));
#13329=CARTESIAN_POINT('Origin',(-3.,0.201909989118576,66.5223738789558));
#13330=CARTESIAN_POINT('',(-2.75,0.201909989118576,66.5223738789558));
#13331=CARTESIAN_POINT('',(-3.,0.201909989118576,66.5223738789558));
#13332=CARTESIAN_POINT('',(-2.75,0.201909989118576,66.5223738789558));
#13333=CARTESIAN_POINT('Origin',(-3.,-1.5334241092205,66.5223738789558));
#13334=CARTESIAN_POINT('',(-2.75,-1.5334241092205,66.5223738789558));
#13335=CARTESIAN_POINT('',(-3.,-1.5334241092205,66.5223738789558));
#13336=CARTESIAN_POINT('',(-2.75,-1.5334241092205,66.5223738789558));
#13337=CARTESIAN_POINT('Origin',(-3.,-1.5334241092205,66.9));
#13338=CARTESIAN_POINT('',(-2.75,-1.5334241092205,66.9));
#13339=CARTESIAN_POINT('',(-3.,-1.5334241092205,66.9));
#13340=CARTESIAN_POINT('',(-2.75,-1.5334241092205,66.9));
#13341=CARTESIAN_POINT('Origin',(-3.,0.625375136733055,66.9));
#13342=CARTESIAN_POINT('',(-2.75,0.625375136733055,66.9));
#13343=CARTESIAN_POINT('',(-3.,0.625375136733055,66.9));
#13344=CARTESIAN_POINT('',(-2.75,0.625375136733055,66.9));
#13345=CARTESIAN_POINT('Origin',(-3.,0.625375136733055,63.7000000715256));
#13346=CARTESIAN_POINT('',(-2.75,0.625375136733055,63.7000000715256));
#13347=CARTESIAN_POINT('',(-3.,0.625375136733055,63.7000000715256));
#13348=CARTESIAN_POINT('',(-2.75,0.625375136733055,63.7000000715256));
#13349=CARTESIAN_POINT('Origin',(-3.,0.201909989118576,63.7000000715256));
#13350=CARTESIAN_POINT('',(-2.75,0.201909989118576,63.7000000715256));
#13351=CARTESIAN_POINT('',(-3.,0.201909989118576,63.7000000715256));
#13352=CARTESIAN_POINT('',(-2.75,0.201909989118576,63.7000000715256));
#13353=CARTESIAN_POINT('Origin',(-3.,0.201909989118576,65.1537516951561));
#13354=CARTESIAN_POINT('',(-2.75,0.201909989118576,65.1537516951561));
#13355=CARTESIAN_POINT('Origin',(-2.75,-0.454024486243725,65.3000000357628));
#13356=CARTESIAN_POINT('Ctrl Pts',(-3.,2.72305563092232,63.6454299330711));
#13357=CARTESIAN_POINT('Ctrl Pts',(-2.75,2.72305563092232,63.6454299330711));
#13358=CARTESIAN_POINT('Ctrl Pts',(-3.,3.17489743232727,63.6454299330711));
#13359=CARTESIAN_POINT('Ctrl Pts',(-2.75,3.17489743232727,63.6454299330711));
#13360=CARTESIAN_POINT('Ctrl Pts',(-3.,3.53069551289082,63.8637107849121));
#13361=CARTESIAN_POINT('Ctrl Pts',(-2.75,3.53069551289082,63.8637107849121));
#13362=CARTESIAN_POINT('',(-2.75,2.72305563092232,63.6454299330711));
#13363=CARTESIAN_POINT('',(-3.,2.72305563092232,63.6454299330711));
#13364=CARTESIAN_POINT('',(-2.75,3.53069551289082,63.8637107849121));
#13365=CARTESIAN_POINT('Ctrl Pts',(-2.75,2.72305563092232,63.6454299330711));
#13366=CARTESIAN_POINT('Ctrl Pts',(-2.75,3.17489743232727,63.6454299330711));
#13367=CARTESIAN_POINT('Ctrl Pts',(-2.75,3.53069551289082,63.8637107849121));
#13368=CARTESIAN_POINT('',(-3.,3.53069551289082,63.8637107849121));
#13369=CARTESIAN_POINT('Ctrl Pts',(-3.,1.94597527384758,63.8429740309715));
#13370=CARTESIAN_POINT('Ctrl Pts',(-2.75,1.94597527384758,63.8429740309715));
#13371=CARTESIAN_POINT('Ctrl Pts',(-3.,2.30613887310028,63.6454299330711));
#13372=CARTESIAN_POINT('Ctrl Pts',(-2.75,2.30613887310028,63.6454299330711));
#13373=CARTESIAN_POINT('Ctrl Pts',(-3.,2.72305563092232,63.6454299330711));
#13374=CARTESIAN_POINT('Ctrl Pts',(-2.75,2.72305563092232,63.6454299330711));
#13375=CARTESIAN_POINT('',(-2.75,1.94597527384758,63.8429740309715));
#13376=CARTESIAN_POINT('',(-3.,1.94597527384758,63.8429740309715));
#13377=CARTESIAN_POINT('Ctrl Pts',(-2.75,1.94597527384758,63.8429740309715));
#13378=CARTESIAN_POINT('Ctrl Pts',(-2.75,2.30613887310028,63.6454299330711));
#13379=CARTESIAN_POINT('Ctrl Pts',(-2.75,2.72305563092232,63.6454299330711));
#13380=CARTESIAN_POINT('Ctrl Pts',(-3.,1.38935878872872,64.4246930122376));
#13381=CARTESIAN_POINT('Ctrl Pts',(-2.75,1.38935878872872,64.4246930122376));
#13382=CARTESIAN_POINT('Ctrl Pts',(-3.,1.58581152558327,64.0405184268951));
#13383=CARTESIAN_POINT('Ctrl Pts',(-2.75,1.58581152558327,64.0405184268951));
#13384=CARTESIAN_POINT('Ctrl Pts',(-3.,1.94597527384758,63.8429740309715));
#13385=CARTESIAN_POINT('Ctrl Pts',(-2.75,1.94597527384758,63.8429740309715));
#13386=CARTESIAN_POINT('',(-2.75,1.38935878872872,64.4246930122376));
#13387=CARTESIAN_POINT('',(-3.,1.38935878872872,64.4246930122376));
#13388=CARTESIAN_POINT('Ctrl Pts',(-2.75,1.38935878872872,64.4246930122376));
#13389=CARTESIAN_POINT('Ctrl Pts',(-2.75,1.58581152558327,64.0405184268951));
#13390=CARTESIAN_POINT('Ctrl Pts',(-2.75,1.94597527384758,63.8429740309715));
#13391=CARTESIAN_POINT('Ctrl Pts',(-3.,1.19290575385094,65.2956342935562));
#13392=CARTESIAN_POINT('Ctrl Pts',(-2.75,1.19290575385094,65.2956342935562));
#13393=CARTESIAN_POINT('Ctrl Pts',(-3.,1.19290575385094,64.80886759758));
#13394=CARTESIAN_POINT('Ctrl Pts',(-2.75,1.19290575385094,64.80886759758));
#13395=CARTESIAN_POINT('Ctrl Pts',(-3.,1.38935878872872,64.4246930122376));
#13396=CARTESIAN_POINT('Ctrl Pts',(-2.75,1.38935878872872,64.4246930122376));
#13397=CARTESIAN_POINT('',(-2.75,1.19290575385094,65.2956342935562));
#13398=CARTESIAN_POINT('',(-3.,1.19290575385094,65.2956342935562));
#13399=CARTESIAN_POINT('Ctrl Pts',(-2.75,1.19290575385094,65.2956342935562));
#13400=CARTESIAN_POINT('Ctrl Pts',(-2.75,1.19290575385094,64.80886759758));
#13401=CARTESIAN_POINT('Ctrl Pts',(-2.75,1.38935878872872,64.4246930122376));
#13402=CARTESIAN_POINT('Ctrl Pts',(-3.,1.37953594326973,66.1545701563358));
#13403=CARTESIAN_POINT('Ctrl Pts',(-2.75,1.37953594326973,66.1545701563358));
#13404=CARTESIAN_POINT('Ctrl Pts',(-3.,1.19290575385094,65.7758526742458));
#13405=CARTESIAN_POINT('Ctrl Pts',(-2.75,1.19290575385094,65.7758526742458));
#13406=CARTESIAN_POINT('Ctrl Pts',(-3.,1.19290575385094,65.2956342935562));
#13407=CARTESIAN_POINT('Ctrl Pts',(-2.75,1.19290575385094,65.2956342935562));
#13408=CARTESIAN_POINT('',(-2.75,1.37953594326973,66.1545701563358));
#13409=CARTESIAN_POINT('',(-3.,1.37953594326973,66.1545701563358));
#13410=CARTESIAN_POINT('Ctrl Pts',(-2.75,1.37953594326973,66.1545701563358));
#13411=CARTESIAN_POINT('Ctrl Pts',(-2.75,1.19290575385094,65.7758526742458));
#13412=CARTESIAN_POINT('Ctrl Pts',(-2.75,1.19290575385094,65.2956342935562));
#13413=CARTESIAN_POINT('Ctrl Pts',(-3.,1.92196443676949,66.7450204730034));
#13414=CARTESIAN_POINT('Ctrl Pts',(-2.75,1.92196443676949,66.7450204730034));
#13415=CARTESIAN_POINT('Ctrl Pts',(-3.,1.56616643071175,66.5332877874374));
#13416=CARTESIAN_POINT('Ctrl Pts',(-2.75,1.56616643071175,66.5332877874374));
#13417=CARTESIAN_POINT('Ctrl Pts',(-3.,1.37953594326973,66.1545701563358));
#13418=CARTESIAN_POINT('Ctrl Pts',(-2.75,1.37953594326973,66.1545701563358));
#13419=CARTESIAN_POINT('',(-2.75,1.92196443676949,66.7450204730034));
#13420=CARTESIAN_POINT('',(-3.,1.92196443676949,66.7450204730034));
#13421=CARTESIAN_POINT('Ctrl Pts',(-2.75,1.92196443676949,66.7450204730034));
#13422=CARTESIAN_POINT('Ctrl Pts',(-2.75,1.56616643071175,66.5332877874374));
#13423=CARTESIAN_POINT('Ctrl Pts',(-2.75,1.37953594326973,66.1545701563358));
#13424=CARTESIAN_POINT('Ctrl Pts',(-3.,2.72087290883064,66.9567531585693));
#13425=CARTESIAN_POINT('Ctrl Pts',(-2.75,2.72087290883064,66.9567531585693));
#13426=CARTESIAN_POINT('Ctrl Pts',(-3.,2.27776229381562,66.9567531585693));
#13427=CARTESIAN_POINT('Ctrl Pts',(-2.75,2.27776229381562,66.9567531585693));
#13428=CARTESIAN_POINT('Ctrl Pts',(-3.,1.92196443676949,66.7450204730034));
#13429=CARTESIAN_POINT('Ctrl Pts',(-2.75,1.92196443676949,66.7450204730034));
#13430=CARTESIAN_POINT('',(-2.75,2.72087290883064,66.9567531585693));
#13431=CARTESIAN_POINT('',(-3.,2.72087290883064,66.9567531585693));
#13432=CARTESIAN_POINT('Ctrl Pts',(-2.75,2.72087290883064,66.9567531585693));
#13433=CARTESIAN_POINT('Ctrl Pts',(-2.75,2.27776229381562,66.9567531585693));
#13434=CARTESIAN_POINT('Ctrl Pts',(-2.75,1.92196443676949,66.7450204730034));
#13435=CARTESIAN_POINT('Ctrl Pts',(-3.,3.82537491619587,66.5060028672218));
#13436=CARTESIAN_POINT('Ctrl Pts',(-2.75,3.82537491619587,66.5060028672218));
#13437=CARTESIAN_POINT('Ctrl Pts',(-3.,3.39754410088063,66.9567531585693));
#13438=CARTESIAN_POINT('Ctrl Pts',(-2.75,3.39754410088063,66.9567531585693));
#13439=CARTESIAN_POINT('Ctrl Pts',(-3.,2.72087290883064,66.9567531585693));
#13440=CARTESIAN_POINT('Ctrl Pts',(-2.75,2.72087290883064,66.9567531585693));
#13441=CARTESIAN_POINT('',(-2.75,3.82537491619587,66.5060028672218));
#13442=CARTESIAN_POINT('',(-3.,3.82537491619587,66.5060028672218));
#13443=CARTESIAN_POINT('Ctrl Pts',(-2.75,3.82537491619587,66.5060028672218));
#13444=CARTESIAN_POINT('Ctrl Pts',(-2.75,3.39754410088063,66.9567531585693));
#13445=CARTESIAN_POINT('Ctrl Pts',(-2.75,2.72087290883064,66.9567531585693));
#13446=CARTESIAN_POINT('Ctrl Pts',(-3.,4.25320571288467,65.2585265278816));
#13447=CARTESIAN_POINT('Ctrl Pts',(-2.75,4.25320571288467,65.2585265278816));
#13448=CARTESIAN_POINT('Ctrl Pts',(-3.,4.25320571288467,66.0552522778511));
#13449=CARTESIAN_POINT('Ctrl Pts',(-2.75,4.25320571288467,66.0552522778511));
#13450=CARTESIAN_POINT('Ctrl Pts',(-3.,3.82537491619587,66.5060028672218));
#13451=CARTESIAN_POINT('Ctrl Pts',(-2.75,3.82537491619587,66.5060028672218));
#13452=CARTESIAN_POINT('',(-2.75,4.25320571288467,65.2585265278816));
#13453=CARTESIAN_POINT('',(-3.,4.25320571288467,65.2585265278816));
#13454=CARTESIAN_POINT('Ctrl Pts',(-2.75,4.25320571288467,65.2585265278816));
#13455=CARTESIAN_POINT('Ctrl Pts',(-2.75,4.25320571288467,66.0552522778511));
#13456=CARTESIAN_POINT('Ctrl Pts',(-2.75,3.82537491619587,66.5060028672218));
#13457=CARTESIAN_POINT('Ctrl Pts',(-3.,4.06984962522984,64.4596180558205));
#13458=CARTESIAN_POINT('Ctrl Pts',(-2.75,4.06984962522984,64.4596180558205));
#13459=CARTESIAN_POINT('Ctrl Pts',(-3.,4.25320571288467,64.8372441768646));
#13460=CARTESIAN_POINT('Ctrl Pts',(-2.75,4.25320571288467,64.8372441768646));
#13461=CARTESIAN_POINT('Ctrl Pts',(-3.,4.25320571288467,65.2585265278816));
#13462=CARTESIAN_POINT('Ctrl Pts',(-2.75,4.25320571288467,65.2585265278816));
#13463=CARTESIAN_POINT('',(-2.75,4.06984962522984,64.4596180558205));
#13464=CARTESIAN_POINT('',(-3.,4.06984962522984,64.4596180558205));
#13465=CARTESIAN_POINT('Ctrl Pts',(-2.75,4.06984962522984,64.4596180558205));
#13466=CARTESIAN_POINT('Ctrl Pts',(-2.75,4.25320571288467,64.8372441768646));
#13467=CARTESIAN_POINT('Ctrl Pts',(-2.75,4.25320571288467,65.2585265278816));
#13468=CARTESIAN_POINT('Ctrl Pts',(-3.,3.53069551289082,63.8637107849121));
#13469=CARTESIAN_POINT('Ctrl Pts',(-2.75,3.53069551289082,63.8637107849121));
#13470=CARTESIAN_POINT('Ctrl Pts',(-3.,3.88649359345436,64.0819919347763));
#13471=CARTESIAN_POINT('Ctrl Pts',(-2.75,3.88649359345436,64.0819919347763));
#13472=CARTESIAN_POINT('Ctrl Pts',(-3.,4.06984962522984,64.4596180558205));
#13473=CARTESIAN_POINT('Ctrl Pts',(-2.75,4.06984962522984,64.4596180558205));
#13474=CARTESIAN_POINT('Ctrl Pts',(-2.75,3.53069551289082,63.8637107849121));
#13475=CARTESIAN_POINT('Ctrl Pts',(-2.75,3.88649359345436,64.0819919347763));
#13476=CARTESIAN_POINT('Ctrl Pts',(-2.75,4.06984962522984,64.4596180558205));
#13477=CARTESIAN_POINT('Origin',(-2.75,2.7230557333678,65.3010915458202));
#13478=CARTESIAN_POINT('Origin',(-3.,16.3103681504726,41.4999999403954));
#13479=CARTESIAN_POINT('',(-2.75,16.3103681504726,41.4999999403954));
#13480=CARTESIAN_POINT('',(-3.,16.3103681504726,41.4999999403954));
#13481=CARTESIAN_POINT('',(-2.75,18.4113232493401,44.6432467103004));
#13482=CARTESIAN_POINT('',(-2.75,16.3103681504726,41.4999999403954));
#13483=CARTESIAN_POINT('',(-3.,18.4113232493401,44.6432467103004));
#13484=CARTESIAN_POINT('Origin',(-3.,15.7673942744732,41.4999999403954));
#13485=CARTESIAN_POINT('',(-2.75,15.7673942744732,41.4999999403954));
#13486=CARTESIAN_POINT('',(-3.,15.7673942744732,41.4999999403954));
#13487=CARTESIAN_POINT('',(-2.75,15.7673942744732,41.4999999403954));
#13488=CARTESIAN_POINT('Origin',(-3.,15.7673942744732,45.5));
#13489=CARTESIAN_POINT('',(-2.75,15.7673942744732,45.5));
#13490=CARTESIAN_POINT('',(-3.,15.7673942744732,45.5));
#13491=CARTESIAN_POINT('',(-2.75,15.7673942744732,45.5));
#13492=CARTESIAN_POINT('Origin',(-3.,16.2748974263668,45.5));
#13493=CARTESIAN_POINT('',(-2.75,16.2748974263668,45.5));
#13494=CARTESIAN_POINT('',(-3.,16.2748974263668,45.5));
#13495=CARTESIAN_POINT('',(-2.75,16.2748974263668,45.5));
#13496=CARTESIAN_POINT('Origin',(-3.,16.2748974263668,42.3594816327095));
#13497=CARTESIAN_POINT('',(-2.75,16.2748974263668,42.3594816327095));
#13498=CARTESIAN_POINT('',(-3.,16.2748974263668,42.3594816327095));
#13499=CARTESIAN_POINT('',(-2.75,16.2748974263668,42.3594816327095));
#13500=CARTESIAN_POINT('Origin',(-3.,18.3758525252342,45.5));
#13501=CARTESIAN_POINT('',(-2.75,18.3758525252342,45.5));
#13502=CARTESIAN_POINT('',(-3.,18.3758525252342,45.5));
#13503=CARTESIAN_POINT('',(-2.75,18.3758525252342,45.5));
#13504=CARTESIAN_POINT('Origin',(-3.,18.9188266247511,45.5));
#13505=CARTESIAN_POINT('',(-2.75,18.9188266247511,45.5));
#13506=CARTESIAN_POINT('',(-3.,18.9188266247511,45.5));
#13507=CARTESIAN_POINT('',(-2.75,18.9188266247511,45.5));
#13508=CARTESIAN_POINT('Origin',(-3.,18.9188266247511,41.4999999403954));
#13509=CARTESIAN_POINT('',(-2.75,18.9188266247511,41.4999999403954));
#13510=CARTESIAN_POINT('',(-3.,18.9188266247511,41.4999999403954));
#13511=CARTESIAN_POINT('',(-2.75,18.9188266247511,41.4999999403954));
#13512=CARTESIAN_POINT('Origin',(-3.,18.4113232493401,41.4999999403954));
#13513=CARTESIAN_POINT('',(-2.75,18.4113232493401,41.4999999403954));
#13514=CARTESIAN_POINT('',(-3.,18.4113232493401,41.4999999403954));
#13515=CARTESIAN_POINT('',(-2.75,18.4113232493401,41.4999999403954));
#13516=CARTESIAN_POINT('Origin',(-3.,18.4113232493401,44.6432467103004));
#13517=CARTESIAN_POINT('',(-2.75,18.4113232493401,44.6432467103004));
#13518=CARTESIAN_POINT('Origin',(-2.75,17.3431104496121,43.4999999701977));
#13519=CARTESIAN_POINT('Ctrl Pts',(-3.,21.5081855356693,41.4317871928215));
#13520=CARTESIAN_POINT('Ctrl Pts',(-2.75,21.5081855356693,41.4317871928215));
#13521=CARTESIAN_POINT('Ctrl Pts',(-3.,22.0729876756668,41.4317871928215));
#13522=CARTESIAN_POINT('Ctrl Pts',(-2.75,22.0729876756668,41.4317871928215));
#13523=CARTESIAN_POINT('Ctrl Pts',(-3.,22.5177353322506,41.7046384811401));
#13524=CARTESIAN_POINT('Ctrl Pts',(-2.75,22.5177353322506,41.7046384811401));
#13525=CARTESIAN_POINT('',(-2.75,21.5081855356693,41.4317871928215));
#13526=CARTESIAN_POINT('',(-3.,21.5081855356693,41.4317871928215));
#13527=CARTESIAN_POINT('',(-2.75,22.5177353322506,41.7046384811401));
#13528=CARTESIAN_POINT('Ctrl Pts',(-2.75,21.5081855356693,41.4317871928215));
#13529=CARTESIAN_POINT('Ctrl Pts',(-2.75,22.0729876756668,41.4317871928215));
#13530=CARTESIAN_POINT('Ctrl Pts',(-2.75,22.5177353322506,41.7046384811401));
#13531=CARTESIAN_POINT('',(-3.,22.5177353322506,41.7046384811401));
#13532=CARTESIAN_POINT('Ctrl Pts',(-3.,20.5368348658085,41.6787176132202));
#13533=CARTESIAN_POINT('Ctrl Pts',(-2.75,20.5368348658085,41.6787176132202));
#13534=CARTESIAN_POINT('Ctrl Pts',(-3.,20.9870394766331,41.4317871928215));
#13535=CARTESIAN_POINT('Ctrl Pts',(-2.75,20.9870394766331,41.4317871928215));
#13536=CARTESIAN_POINT('Ctrl Pts',(-3.,21.5081855356693,41.4317871928215));
#13537=CARTESIAN_POINT('Ctrl Pts',(-2.75,21.5081855356693,41.4317871928215));
#13538=CARTESIAN_POINT('',(-2.75,20.5368348658085,41.6787176132202));
#13539=CARTESIAN_POINT('',(-3.,20.5368348658085,41.6787176132202));
#13540=CARTESIAN_POINT('Ctrl Pts',(-2.75,20.5368348658085,41.6787176132202));
#13541=CARTESIAN_POINT('Ctrl Pts',(-2.75,20.9870394766331,41.4317871928215));
#13542=CARTESIAN_POINT('Ctrl Pts',(-2.75,21.5081855356693,41.4317871928215));
#13543=CARTESIAN_POINT('Ctrl Pts',(-3.,19.8410638868809,42.4058662652969));
#13544=CARTESIAN_POINT('Ctrl Pts',(-2.75,19.8410638868809,42.4058662652969));
#13545=CARTESIAN_POINT('Ctrl Pts',(-3.,20.0866302549839,41.9256480336189));
#13546=CARTESIAN_POINT('Ctrl Pts',(-2.75,20.0866302549839,41.9256480336189));
#13547=CARTESIAN_POINT('Ctrl Pts',(-3.,20.5368348658085,41.6787176132202));
#13548=CARTESIAN_POINT('Ctrl Pts',(-2.75,20.5368348658085,41.6787176132202));
#13549=CARTESIAN_POINT('',(-2.75,19.8410638868809,42.4058662652969));
#13550=CARTESIAN_POINT('',(-3.,19.8410638868809,42.4058662652969));
#13551=CARTESIAN_POINT('Ctrl Pts',(-2.75,19.8410638868809,42.4058662652969));
#13552=CARTESIAN_POINT('Ctrl Pts',(-2.75,20.0866302549839,41.9256480336189));
#13553=CARTESIAN_POINT('Ctrl Pts',(-2.75,20.5368348658085,41.6787176132202));
#13554=CARTESIAN_POINT('Ctrl Pts',(-3.,19.5954978168011,43.4945430159569));
#13555=CARTESIAN_POINT('Ctrl Pts',(-2.75,19.5954978168011,43.4945430159569));
#13556=CARTESIAN_POINT('Ctrl Pts',(-3.,19.5954978168011,42.8860844969749));
#13557=CARTESIAN_POINT('Ctrl Pts',(-2.75,19.5954978168011,42.8860844969749));
#13558=CARTESIAN_POINT('Ctrl Pts',(-3.,19.8410638868809,42.4058662652969));
#13559=CARTESIAN_POINT('Ctrl Pts',(-2.75,19.8410638868809,42.4058662652969));
#13560=CARTESIAN_POINT('',(-2.75,19.5954978168011,43.4945430159569));
#13561=CARTESIAN_POINT('',(-3.,19.5954978168011,43.4945430159569));
#13562=CARTESIAN_POINT('Ctrl Pts',(-2.75,19.5954978168011,43.4945430159569));
#13563=CARTESIAN_POINT('Ctrl Pts',(-2.75,19.5954978168011,42.8860844969749));
#13564=CARTESIAN_POINT('Ctrl Pts',(-2.75,19.8410638868809,42.4058662652969));
#13565=CARTESIAN_POINT('Ctrl Pts',(-3.,19.8287856280804,44.5682128071785));
#13566=CARTESIAN_POINT('Ctrl Pts',(-2.75,19.8287856280804,44.5682128071785));
#13567=CARTESIAN_POINT('Ctrl Pts',(-3.,19.5954978168011,44.0948157310486));
#13568=CARTESIAN_POINT('Ctrl Pts',(-2.75,19.5954978168011,44.0948157310486));
#13569=CARTESIAN_POINT('Ctrl Pts',(-3.,19.5954978168011,43.4945430159569));
#13570=CARTESIAN_POINT('Ctrl Pts',(-2.75,19.5954978168011,43.4945430159569));
#13571=CARTESIAN_POINT('',(-2.75,19.8287856280804,44.5682128071785));
#13572=CARTESIAN_POINT('',(-3.,19.8287856280804,44.5682128071785));
#13573=CARTESIAN_POINT('Ctrl Pts',(-2.75,19.8287856280804,44.5682128071785));
#13574=CARTESIAN_POINT('Ctrl Pts',(-2.75,19.5954978168011,44.0948157310486));
#13575=CARTESIAN_POINT('Ctrl Pts',(-2.75,19.5954978168011,43.4945430159569));
#13576=CARTESIAN_POINT('Ctrl Pts',(-3.,20.5068212449551,45.30627566576));
#13577=CARTESIAN_POINT('Ctrl Pts',(-2.75,20.5068212449551,45.30627566576));
#13578=CARTESIAN_POINT('Ctrl Pts',(-3.,20.0620734393597,45.0416098833084));
#13579=CARTESIAN_POINT('Ctrl Pts',(-2.75,20.0620734393597,45.0416098833084));
#13580=CARTESIAN_POINT('Ctrl Pts',(-3.,19.8287856280804,44.5682128071785));
#13581=CARTESIAN_POINT('Ctrl Pts',(-2.75,19.8287856280804,44.5682128071785));
#13582=CARTESIAN_POINT('',(-2.75,20.5068212449551,45.30627566576));
#13583=CARTESIAN_POINT('',(-3.,20.5068212449551,45.30627566576));
#13584=CARTESIAN_POINT('Ctrl Pts',(-2.75,20.5068212449551,45.30627566576));
#13585=CARTESIAN_POINT('Ctrl Pts',(-2.75,20.0620734393597,45.0416098833084));
#13586=CARTESIAN_POINT('Ctrl Pts',(-2.75,19.8287856280804,44.5682128071785));
#13587=CARTESIAN_POINT('Ctrl Pts',(-3.,21.5054569840431,45.5709411501884));
#13588=CARTESIAN_POINT('Ctrl Pts',(-2.75,21.5054569840431,45.5709411501884));
#13589=CARTESIAN_POINT('Ctrl Pts',(-3.,20.9515687525272,45.5709411501884));
#13590=CARTESIAN_POINT('Ctrl Pts',(-2.75,20.9515687525272,45.5709411501884));
#13591=CARTESIAN_POINT('Ctrl Pts',(-3.,20.5068212449551,45.30627566576));
#13592=CARTESIAN_POINT('Ctrl Pts',(-2.75,20.5068212449551,45.30627566576));
#13593=CARTESIAN_POINT('',(-2.75,21.5054569840431,45.5709411501884));
#13594=CARTESIAN_POINT('',(-3.,21.5054569840431,45.5709411501884));
#13595=CARTESIAN_POINT('Ctrl Pts',(-2.75,21.5054569840431,45.5709411501884));
#13596=CARTESIAN_POINT('Ctrl Pts',(-2.75,20.9515687525272,45.5709411501884));
#13597=CARTESIAN_POINT('Ctrl Pts',(-2.75,20.5068212449551,45.30627566576));
#13598=CARTESIAN_POINT('Ctrl Pts',(-3.,22.8860845863819,45.0075035095215));
#13599=CARTESIAN_POINT('Ctrl Pts',(-2.75,22.8860845863819,45.0075035095215));
#13600=CARTESIAN_POINT('Ctrl Pts',(-3.,22.3512960672379,45.5709411501884));
#13601=CARTESIAN_POINT('Ctrl Pts',(-2.75,22.3512960672379,45.5709411501884));
#13602=CARTESIAN_POINT('Ctrl Pts',(-3.,21.5054569840431,45.5709411501884));
#13603=CARTESIAN_POINT('Ctrl Pts',(-2.75,21.5054569840431,45.5709411501884));
#13604=CARTESIAN_POINT('',(-2.75,22.8860845863819,45.0075035095215));
#13605=CARTESIAN_POINT('',(-3.,22.8860845863819,45.0075035095215));
#13606=CARTESIAN_POINT('Ctrl Pts',(-2.75,22.8860845863819,45.0075035095215));
#13607=CARTESIAN_POINT('Ctrl Pts',(-2.75,22.3512960672379,45.5709411501884));
#13608=CARTESIAN_POINT('Ctrl Pts',(-2.75,21.5054569840431,45.5709411501884));
#13609=CARTESIAN_POINT('Ctrl Pts',(-3.,23.4208730682731,43.4481580853462));
#13610=CARTESIAN_POINT('Ctrl Pts',(-2.75,23.4208730682731,43.4481580853462));
#13611=CARTESIAN_POINT('Ctrl Pts',(-3.,23.4208730682731,44.4440655708313));
#13612=CARTESIAN_POINT('Ctrl Pts',(-2.75,23.4208730682731,44.4440655708313));
#13613=CARTESIAN_POINT('Ctrl Pts',(-3.,22.8860845863819,45.0075035095215));
#13614=CARTESIAN_POINT('Ctrl Pts',(-2.75,22.8860845863819,45.0075035095215));
#13615=CARTESIAN_POINT('',(-2.75,23.4208730682731,43.4481580853462));
#13616=CARTESIAN_POINT('',(-3.,23.4208730682731,43.4481580853462));
#13617=CARTESIAN_POINT('Ctrl Pts',(-2.75,23.4208730682731,43.4481580853462));
#13618=CARTESIAN_POINT('Ctrl Pts',(-2.75,23.4208730682731,44.4440655708313));
#13619=CARTESIAN_POINT('Ctrl Pts',(-2.75,22.8860845863819,45.0075035095215));
#13620=CARTESIAN_POINT('Ctrl Pts',(-3.,23.1916779726744,42.4495224952698));
#13621=CARTESIAN_POINT('Ctrl Pts',(-2.75,23.1916779726744,42.4495224952698));
#13622=CARTESIAN_POINT('Ctrl Pts',(-3.,23.4208730682731,42.9215552210808));
#13623=CARTESIAN_POINT('Ctrl Pts',(-2.75,23.4208730682731,42.9215552210808));
#13624=CARTESIAN_POINT('Ctrl Pts',(-3.,23.4208730682731,43.4481580853462));
#13625=CARTESIAN_POINT('Ctrl Pts',(-2.75,23.4208730682731,43.4481580853462));
#13626=CARTESIAN_POINT('',(-2.75,23.1916779726744,42.4495224952698));
#13627=CARTESIAN_POINT('',(-3.,23.1916779726744,42.4495224952698));
#13628=CARTESIAN_POINT('Ctrl Pts',(-2.75,23.1916779726744,42.4495224952698));
#13629=CARTESIAN_POINT('Ctrl Pts',(-2.75,23.4208730682731,42.9215552210808));
#13630=CARTESIAN_POINT('Ctrl Pts',(-2.75,23.4208730682731,43.4481580853462));
#13631=CARTESIAN_POINT('Ctrl Pts',(-3.,22.5177353322506,41.7046384811401));
#13632=CARTESIAN_POINT('Ctrl Pts',(-2.75,22.5177353322506,41.7046384811401));
#13633=CARTESIAN_POINT('Ctrl Pts',(-3.,22.9624829143286,41.9774897694588));
#13634=CARTESIAN_POINT('Ctrl Pts',(-2.75,22.9624829143286,41.9774897694588));
#13635=CARTESIAN_POINT('Ctrl Pts',(-3.,23.1916779726744,42.4495224952698));
#13636=CARTESIAN_POINT('Ctrl Pts',(-2.75,23.1916779726744,42.4495224952698));
#13637=CARTESIAN_POINT('Ctrl Pts',(-2.75,22.5177353322506,41.7046384811401));
#13638=CARTESIAN_POINT('Ctrl Pts',(-2.75,22.9624829143286,41.9774897694588));
#13639=CARTESIAN_POINT('Ctrl Pts',(-2.75,23.1916779726744,42.4495224952698));
#13640=CARTESIAN_POINT('Origin',(-2.75,21.5081854425371,43.501364171505));
#13641=CARTESIAN_POINT('Origin',(-3.,-22.6896318495274,41.4999999403954));
#13642=CARTESIAN_POINT('',(-2.75,-22.6896318495274,41.4999999403954));
#13643=CARTESIAN_POINT('',(-3.,-22.6896318495274,41.4999999403954));
#13644=CARTESIAN_POINT('',(-2.75,-20.5886767506599,44.6432467103004));
#13645=CARTESIAN_POINT('',(-2.75,-22.6896318495274,41.4999999403954));
#13646=CARTESIAN_POINT('',(-3.,-20.5886767506599,44.6432467103004));
#13647=CARTESIAN_POINT('Origin',(-3.,-23.2326057255268,41.4999999403954));
#13648=CARTESIAN_POINT('',(-2.75,-23.2326057255268,41.4999999403954));
#13649=CARTESIAN_POINT('',(-3.,-23.2326057255268,41.4999999403954));
#13650=CARTESIAN_POINT('',(-2.75,-23.2326057255268,41.4999999403954));
#13651=CARTESIAN_POINT('Origin',(-3.,-23.2326057255268,45.5));
#13652=CARTESIAN_POINT('',(-2.75,-23.2326057255268,45.5));
#13653=CARTESIAN_POINT('',(-3.,-23.2326057255268,45.5));
#13654=CARTESIAN_POINT('',(-2.75,-23.2326057255268,45.5));
#13655=CARTESIAN_POINT('Origin',(-3.,-22.7251025736332,45.5));
#13656=CARTESIAN_POINT('',(-2.75,-22.7251025736332,45.5));
#13657=CARTESIAN_POINT('',(-3.,-22.7251025736332,45.5));
#13658=CARTESIAN_POINT('',(-2.75,-22.7251025736332,45.5));
#13659=CARTESIAN_POINT('Origin',(-3.,-22.7251025736332,42.3594816327095));
#13660=CARTESIAN_POINT('',(-2.75,-22.7251025736332,42.3594816327095));
#13661=CARTESIAN_POINT('',(-3.,-22.7251025736332,42.3594816327095));
#13662=CARTESIAN_POINT('',(-2.75,-22.7251025736332,42.3594816327095));
#13663=CARTESIAN_POINT('Origin',(-3.,-20.6241474747658,45.5));
#13664=CARTESIAN_POINT('',(-2.75,-20.6241474747658,45.5));
#13665=CARTESIAN_POINT('',(-3.,-20.6241474747658,45.5));
#13666=CARTESIAN_POINT('',(-2.75,-20.6241474747658,45.5));
#13667=CARTESIAN_POINT('Origin',(-3.,-20.0811733752489,45.5));
#13668=CARTESIAN_POINT('',(-2.75,-20.0811733752489,45.5));
#13669=CARTESIAN_POINT('',(-3.,-20.0811733752489,45.5));
#13670=CARTESIAN_POINT('',(-2.75,-20.0811733752489,45.5));
#13671=CARTESIAN_POINT('Origin',(-3.,-20.0811733752489,41.4999999403954));
#13672=CARTESIAN_POINT('',(-2.75,-20.0811733752489,41.4999999403954));
#13673=CARTESIAN_POINT('',(-3.,-20.0811733752489,41.4999999403954));
#13674=CARTESIAN_POINT('',(-2.75,-20.0811733752489,41.4999999403954));
#13675=CARTESIAN_POINT('Origin',(-3.,-20.5886767506599,41.4999999403954));
#13676=CARTESIAN_POINT('',(-2.75,-20.5886767506599,41.4999999403954));
#13677=CARTESIAN_POINT('',(-3.,-20.5886767506599,41.4999999403954));
#13678=CARTESIAN_POINT('',(-2.75,-20.5886767506599,41.4999999403954));
#13679=CARTESIAN_POINT('Origin',(-3.,-20.5886767506599,44.6432467103004));
#13680=CARTESIAN_POINT('',(-2.75,-20.5886767506599,44.6432467103004));
#13681=CARTESIAN_POINT('Origin',(-2.75,-21.6568895503879,43.4999999701977));
#13682=CARTESIAN_POINT('Ctrl Pts',(-3.,-17.4918144643307,41.4317871928215));
#13683=CARTESIAN_POINT('Ctrl Pts',(-2.75,-17.4918144643307,41.4317871928215));
#13684=CARTESIAN_POINT('Ctrl Pts',(-3.,-16.9270123243332,41.4317871928215));
#13685=CARTESIAN_POINT('Ctrl Pts',(-2.75,-16.9270123243332,41.4317871928215));
#13686=CARTESIAN_POINT('Ctrl Pts',(-3.,-16.4822646677494,41.7046384811401));
#13687=CARTESIAN_POINT('Ctrl Pts',(-2.75,-16.4822646677494,41.7046384811401));
#13688=CARTESIAN_POINT('',(-2.75,-17.4918144643307,41.4317871928215));
#13689=CARTESIAN_POINT('',(-3.,-17.4918144643307,41.4317871928215));
#13690=CARTESIAN_POINT('',(-2.75,-16.4822646677494,41.7046384811401));
#13691=CARTESIAN_POINT('Ctrl Pts',(-2.75,-17.4918144643307,41.4317871928215));
#13692=CARTESIAN_POINT('Ctrl Pts',(-2.75,-16.9270123243332,41.4317871928215));
#13693=CARTESIAN_POINT('Ctrl Pts',(-2.75,-16.4822646677494,41.7046384811401));
#13694=CARTESIAN_POINT('',(-3.,-16.4822646677494,41.7046384811401));
#13695=CARTESIAN_POINT('Ctrl Pts',(-3.,-18.4631651341915,41.6787176132202));
#13696=CARTESIAN_POINT('Ctrl Pts',(-2.75,-18.4631651341915,41.6787176132202));
#13697=CARTESIAN_POINT('Ctrl Pts',(-3.,-18.0129605233669,41.4317871928215));
#13698=CARTESIAN_POINT('Ctrl Pts',(-2.75,-18.0129605233669,41.4317871928215));
#13699=CARTESIAN_POINT('Ctrl Pts',(-3.,-17.4918144643307,41.4317871928215));
#13700=CARTESIAN_POINT('Ctrl Pts',(-2.75,-17.4918144643307,41.4317871928215));
#13701=CARTESIAN_POINT('',(-2.75,-18.4631651341915,41.6787176132202));
#13702=CARTESIAN_POINT('',(-3.,-18.4631651341915,41.6787176132202));
#13703=CARTESIAN_POINT('Ctrl Pts',(-2.75,-18.4631651341915,41.6787176132202));
#13704=CARTESIAN_POINT('Ctrl Pts',(-2.75,-18.0129605233669,41.4317871928215));
#13705=CARTESIAN_POINT('Ctrl Pts',(-2.75,-17.4918144643307,41.4317871928215));
#13706=CARTESIAN_POINT('Ctrl Pts',(-3.,-19.1589361131191,42.4058662652969));
#13707=CARTESIAN_POINT('Ctrl Pts',(-2.75,-19.1589361131191,42.4058662652969));
#13708=CARTESIAN_POINT('Ctrl Pts',(-3.,-18.9133697450161,41.9256480336189));
#13709=CARTESIAN_POINT('Ctrl Pts',(-2.75,-18.9133697450161,41.9256480336189));
#13710=CARTESIAN_POINT('Ctrl Pts',(-3.,-18.4631651341915,41.6787176132202));
#13711=CARTESIAN_POINT('Ctrl Pts',(-2.75,-18.4631651341915,41.6787176132202));
#13712=CARTESIAN_POINT('',(-2.75,-19.1589361131191,42.4058662652969));
#13713=CARTESIAN_POINT('',(-3.,-19.1589361131191,42.4058662652969));
#13714=CARTESIAN_POINT('Ctrl Pts',(-2.75,-19.1589361131191,42.4058662652969));
#13715=CARTESIAN_POINT('Ctrl Pts',(-2.75,-18.9133697450161,41.9256480336189));
#13716=CARTESIAN_POINT('Ctrl Pts',(-2.75,-18.4631651341915,41.6787176132202));
#13717=CARTESIAN_POINT('Ctrl Pts',(-3.,-19.4045021831989,43.4945430159569));
#13718=CARTESIAN_POINT('Ctrl Pts',(-2.75,-19.4045021831989,43.4945430159569));
#13719=CARTESIAN_POINT('Ctrl Pts',(-3.,-19.4045021831989,42.8860844969749));
#13720=CARTESIAN_POINT('Ctrl Pts',(-2.75,-19.4045021831989,42.8860844969749));
#13721=CARTESIAN_POINT('Ctrl Pts',(-3.,-19.1589361131191,42.4058662652969));
#13722=CARTESIAN_POINT('Ctrl Pts',(-2.75,-19.1589361131191,42.4058662652969));
#13723=CARTESIAN_POINT('',(-2.75,-19.4045021831989,43.4945430159569));
#13724=CARTESIAN_POINT('',(-3.,-19.4045021831989,43.4945430159569));
#13725=CARTESIAN_POINT('Ctrl Pts',(-2.75,-19.4045021831989,43.4945430159569));
#13726=CARTESIAN_POINT('Ctrl Pts',(-2.75,-19.4045021831989,42.8860844969749));
#13727=CARTESIAN_POINT('Ctrl Pts',(-2.75,-19.1589361131191,42.4058662652969));
#13728=CARTESIAN_POINT('Ctrl Pts',(-3.,-19.1712143719196,44.5682128071785));
#13729=CARTESIAN_POINT('Ctrl Pts',(-2.75,-19.1712143719196,44.5682128071785));
#13730=CARTESIAN_POINT('Ctrl Pts',(-3.,-19.4045021831989,44.0948157310486));
#13731=CARTESIAN_POINT('Ctrl Pts',(-2.75,-19.4045021831989,44.0948157310486));
#13732=CARTESIAN_POINT('Ctrl Pts',(-3.,-19.4045021831989,43.4945430159569));
#13733=CARTESIAN_POINT('Ctrl Pts',(-2.75,-19.4045021831989,43.4945430159569));
#13734=CARTESIAN_POINT('',(-2.75,-19.1712143719196,44.5682128071785));
#13735=CARTESIAN_POINT('',(-3.,-19.1712143719196,44.5682128071785));
#13736=CARTESIAN_POINT('Ctrl Pts',(-2.75,-19.1712143719196,44.5682128071785));
#13737=CARTESIAN_POINT('Ctrl Pts',(-2.75,-19.4045021831989,44.0948157310486));
#13738=CARTESIAN_POINT('Ctrl Pts',(-2.75,-19.4045021831989,43.4945430159569));
#13739=CARTESIAN_POINT('Ctrl Pts',(-3.,-18.4931787550449,45.30627566576));
#13740=CARTESIAN_POINT('Ctrl Pts',(-2.75,-18.4931787550449,45.30627566576));
#13741=CARTESIAN_POINT('Ctrl Pts',(-3.,-18.9379265606403,45.0416098833084));
#13742=CARTESIAN_POINT('Ctrl Pts',(-2.75,-18.9379265606403,45.0416098833084));
#13743=CARTESIAN_POINT('Ctrl Pts',(-3.,-19.1712143719196,44.5682128071785));
#13744=CARTESIAN_POINT('Ctrl Pts',(-2.75,-19.1712143719196,44.5682128071785));
#13745=CARTESIAN_POINT('',(-2.75,-18.4931787550449,45.30627566576));
#13746=CARTESIAN_POINT('',(-3.,-18.4931787550449,45.30627566576));
#13747=CARTESIAN_POINT('Ctrl Pts',(-2.75,-18.4931787550449,45.30627566576));
#13748=CARTESIAN_POINT('Ctrl Pts',(-2.75,-18.9379265606403,45.0416098833084));
#13749=CARTESIAN_POINT('Ctrl Pts',(-2.75,-19.1712143719196,44.5682128071785));
#13750=CARTESIAN_POINT('Ctrl Pts',(-3.,-17.4945430159569,45.5709411501884));
#13751=CARTESIAN_POINT('Ctrl Pts',(-2.75,-17.4945430159569,45.5709411501884));
#13752=CARTESIAN_POINT('Ctrl Pts',(-3.,-18.0484312474728,45.5709411501884));
#13753=CARTESIAN_POINT('Ctrl Pts',(-2.75,-18.0484312474728,45.5709411501884));
#13754=CARTESIAN_POINT('Ctrl Pts',(-3.,-18.4931787550449,45.30627566576));
#13755=CARTESIAN_POINT('Ctrl Pts',(-2.75,-18.4931787550449,45.30627566576));
#13756=CARTESIAN_POINT('',(-2.75,-17.4945430159569,45.5709411501884));
#13757=CARTESIAN_POINT('',(-3.,-17.4945430159569,45.5709411501884));
#13758=CARTESIAN_POINT('Ctrl Pts',(-2.75,-17.4945430159569,45.5709411501884));
#13759=CARTESIAN_POINT('Ctrl Pts',(-2.75,-18.0484312474728,45.5709411501884));
#13760=CARTESIAN_POINT('Ctrl Pts',(-2.75,-18.4931787550449,45.30627566576));
#13761=CARTESIAN_POINT('Ctrl Pts',(-3.,-16.1139154136181,45.0075035095215));
#13762=CARTESIAN_POINT('Ctrl Pts',(-2.75,-16.1139154136181,45.0075035095215));
#13763=CARTESIAN_POINT('Ctrl Pts',(-3.,-16.6487039327621,45.5709411501884));
#13764=CARTESIAN_POINT('Ctrl Pts',(-2.75,-16.6487039327621,45.5709411501884));
#13765=CARTESIAN_POINT('Ctrl Pts',(-3.,-17.4945430159569,45.5709411501884));
#13766=CARTESIAN_POINT('Ctrl Pts',(-2.75,-17.4945430159569,45.5709411501884));
#13767=CARTESIAN_POINT('',(-2.75,-16.1139154136181,45.0075035095215));
#13768=CARTESIAN_POINT('',(-3.,-16.1139154136181,45.0075035095215));
#13769=CARTESIAN_POINT('Ctrl Pts',(-2.75,-16.1139154136181,45.0075035095215));
#13770=CARTESIAN_POINT('Ctrl Pts',(-2.75,-16.6487039327621,45.5709411501884));
#13771=CARTESIAN_POINT('Ctrl Pts',(-2.75,-17.4945430159569,45.5709411501884));
#13772=CARTESIAN_POINT('Ctrl Pts',(-3.,-15.5791269317269,43.4481580853462));
#13773=CARTESIAN_POINT('Ctrl Pts',(-2.75,-15.5791269317269,43.4481580853462));
#13774=CARTESIAN_POINT('Ctrl Pts',(-3.,-15.5791269317269,44.4440655708313));
#13775=CARTESIAN_POINT('Ctrl Pts',(-2.75,-15.5791269317269,44.4440655708313));
#13776=CARTESIAN_POINT('Ctrl Pts',(-3.,-16.1139154136181,45.0075035095215));
#13777=CARTESIAN_POINT('Ctrl Pts',(-2.75,-16.1139154136181,45.0075035095215));
#13778=CARTESIAN_POINT('',(-2.75,-15.5791269317269,43.4481580853462));
#13779=CARTESIAN_POINT('',(-3.,-15.5791269317269,43.4481580853462));
#13780=CARTESIAN_POINT('Ctrl Pts',(-2.75,-15.5791269317269,43.4481580853462));
#13781=CARTESIAN_POINT('Ctrl Pts',(-2.75,-15.5791269317269,44.4440655708313));
#13782=CARTESIAN_POINT('Ctrl Pts',(-2.75,-16.1139154136181,45.0075035095215));
#13783=CARTESIAN_POINT('Ctrl Pts',(-3.,-15.8083220273256,42.4495224952698));
#13784=CARTESIAN_POINT('Ctrl Pts',(-2.75,-15.8083220273256,42.4495224952698));
#13785=CARTESIAN_POINT('Ctrl Pts',(-3.,-15.5791269317269,42.9215552210808));
#13786=CARTESIAN_POINT('Ctrl Pts',(-2.75,-15.5791269317269,42.9215552210808));
#13787=CARTESIAN_POINT('Ctrl Pts',(-3.,-15.5791269317269,43.4481580853462));
#13788=CARTESIAN_POINT('Ctrl Pts',(-2.75,-15.5791269317269,43.4481580853462));
#13789=CARTESIAN_POINT('',(-2.75,-15.8083220273256,42.4495224952698));
#13790=CARTESIAN_POINT('',(-3.,-15.8083220273256,42.4495224952698));
#13791=CARTESIAN_POINT('Ctrl Pts',(-2.75,-15.8083220273256,42.4495224952698));
#13792=CARTESIAN_POINT('Ctrl Pts',(-2.75,-15.5791269317269,42.9215552210808));
#13793=CARTESIAN_POINT('Ctrl Pts',(-2.75,-15.5791269317269,43.4481580853462));
#13794=CARTESIAN_POINT('Ctrl Pts',(-3.,-16.4822646677494,41.7046384811401));
#13795=CARTESIAN_POINT('Ctrl Pts',(-2.75,-16.4822646677494,41.7046384811401));
#13796=CARTESIAN_POINT('Ctrl Pts',(-3.,-16.0375170856714,41.9774897694588));
#13797=CARTESIAN_POINT('Ctrl Pts',(-2.75,-16.0375170856714,41.9774897694588));
#13798=CARTESIAN_POINT('Ctrl Pts',(-3.,-15.8083220273256,42.4495224952698));
#13799=CARTESIAN_POINT('Ctrl Pts',(-2.75,-15.8083220273256,42.4495224952698));
#13800=CARTESIAN_POINT('Ctrl Pts',(-2.75,-16.4822646677494,41.7046384811401));
#13801=CARTESIAN_POINT('Ctrl Pts',(-2.75,-16.0375170856714,41.9774897694588));
#13802=CARTESIAN_POINT('Ctrl Pts',(-2.75,-15.8083220273256,42.4495224952698));
#13803=CARTESIAN_POINT('Origin',(-2.75,-17.4918145574629,43.501364171505));
#13804=CARTESIAN_POINT('Origin',(-3.,25.,66.5));
#13805=CARTESIAN_POINT('',(-3.,25.,68.2));
#13806=CARTESIAN_POINT('Origin',(-3.,-25.,26.5));
#13807=CARTESIAN_POINT('',(-3.,-25.,28.2));
#13808=CARTESIAN_POINT('Origin',(-3.,-25.,66.5));
#13809=CARTESIAN_POINT('',(-3.,-25.,68.2));
#13810=CARTESIAN_POINT('Origin',(-3.,25.,26.5));
#13811=CARTESIAN_POINT('',(-3.,25.,28.2));
#13812=CARTESIAN_POINT('Origin',(-3.,0.,47.5));
#13813=CARTESIAN_POINT('',(-3.,-7.9602041944578E-16,54.));
#13814=CARTESIAN_POINT('Origin',(0.,25.1,26.5));
#13815=CARTESIAN_POINT('',(0.,25.1,22.5));
#13816=CARTESIAN_POINT('Origin',(0.,-25.1,26.5));
#13817=CARTESIAN_POINT('',(0.,-25.1,22.5));
#13818=CARTESIAN_POINT('Origin',(0.,29.1,22.5));
#13819=CARTESIAN_POINT('',(0.,0.,0.));
#13820=CARTESIAN_POINT('Origin',(100.1,-29.,58.575));
#13821=CARTESIAN_POINT('',(100.,-28.9,26.5));
#13822=CARTESIAN_POINT('',(100.2,-29.1,26.5));
#13823=CARTESIAN_POINT('',(100.,-28.9,26.5));
#13824=CARTESIAN_POINT('',(100.2,-29.1,66.6));
#13825=CARTESIAN_POINT('',(100.2,-29.1,58.575));
#13826=CARTESIAN_POINT('',(100.,-28.9,66.6));
#13827=CARTESIAN_POINT('',(100.2,-29.1,66.6));
#13828=CARTESIAN_POINT('',(100.,-28.9,58.575));
#13829=CARTESIAN_POINT('Origin',(100.1,-25.1,26.5));
#13830=CARTESIAN_POINT('',(100.,-25.1,22.7));
#13831=CARTESIAN_POINT('',(100.2,-25.1,22.5));
#13832=CARTESIAN_POINT('',(100.,-25.1,22.7));
#13833=CARTESIAN_POINT('Origin',(100.2,-25.1,26.5));
#13834=CARTESIAN_POINT('Origin',(100.,-25.1,26.5));
#13835=CARTESIAN_POINT('Origin',(100.1,-14.55,22.6));
#13836=CARTESIAN_POINT('',(100.,25.1,22.7));
#13837=CARTESIAN_POINT('',(100.2,25.1,22.5));
#13838=CARTESIAN_POINT('',(100.,25.1,22.7));
#13839=CARTESIAN_POINT('',(100.2,-14.55,22.5));
#13840=CARTESIAN_POINT('',(100.,-14.55,22.7));
#13841=CARTESIAN_POINT('Origin',(100.1,25.1,26.5));
#13842=CARTESIAN_POINT('',(100.,28.9,26.5));
#13843=CARTESIAN_POINT('',(100.2,29.1,26.5));
#13844=CARTESIAN_POINT('',(100.,28.9,26.5));
#13845=CARTESIAN_POINT('Origin',(100.2,25.1,26.5));
#13846=CARTESIAN_POINT('Origin',(100.,25.1,26.5));
#13847=CARTESIAN_POINT('Origin',(100.1,29.,34.525));
#13848=CARTESIAN_POINT('',(100.,28.9,66.6));
#13849=CARTESIAN_POINT('',(100.2,29.1,66.6));
#13850=CARTESIAN_POINT('',(100.,28.9,66.6));
#13851=CARTESIAN_POINT('',(100.2,29.1,34.525));
#13852=CARTESIAN_POINT('',(100.,28.9,34.525));
#13853=CARTESIAN_POINT('Origin',(100.1,25.1,66.6));
#13854=CARTESIAN_POINT('',(100.,25.1,70.4));
#13855=CARTESIAN_POINT('',(100.2,25.1,70.6));
#13856=CARTESIAN_POINT('',(100.,25.1,70.4));
#13857=CARTESIAN_POINT('Origin',(100.2,25.1,66.6));
#13858=CARTESIAN_POINT('Origin',(100.,25.1,66.6));
#13859=CARTESIAN_POINT('Origin',(100.1,14.55,70.5));
#13860=CARTESIAN_POINT('',(100.,-25.1,70.4));
#13861=CARTESIAN_POINT('',(100.2,-25.1,70.6));
#13862=CARTESIAN_POINT('',(100.,-25.1,70.4));
#13863=CARTESIAN_POINT('',(100.2,14.55,70.6));
#13864=CARTESIAN_POINT('',(100.,14.55,70.4));
#13865=CARTESIAN_POINT('Origin',(100.1,-25.1,66.6));
#13866=CARTESIAN_POINT('Origin',(100.2,-25.1,66.6));
#13867=CARTESIAN_POINT('Origin',(100.,-25.1,66.6));
#13868=CARTESIAN_POINT('Origin',(100.,25.1,66.6));
#13869=CARTESIAN_POINT('',(102.8,25.1,70.6));
#13870=CARTESIAN_POINT('',(100.,25.1,70.6));
#13871=CARTESIAN_POINT('',(102.8,29.1,66.6));
#13872=CARTESIAN_POINT('Origin',(102.8,25.1,66.6));
#13873=CARTESIAN_POINT('',(100.,29.1,66.6));
#13874=CARTESIAN_POINT('Origin',(100.,29.1,70.6));
#13875=CARTESIAN_POINT('',(102.8,-25.1,70.6));
#13876=CARTESIAN_POINT('',(100.,-25.1,70.6));
#13877=CARTESIAN_POINT('',(102.8,14.55,70.6));
#13878=CARTESIAN_POINT('Origin',(100.,-25.1,66.6));
#13879=CARTESIAN_POINT('',(102.8,-29.1,66.6));
#13880=CARTESIAN_POINT('',(100.,-29.1,66.6));
#13881=CARTESIAN_POINT('Origin',(102.8,-25.1,66.6));
#13882=CARTESIAN_POINT('Origin',(100.,-29.1,70.6));
#13883=CARTESIAN_POINT('',(102.8,-29.1,26.5));
#13884=CARTESIAN_POINT('',(100.,-29.1,26.5));
#13885=CARTESIAN_POINT('',(102.8,-29.1,58.575));
#13886=CARTESIAN_POINT('Origin',(100.,0.,46.55));
#13887=CARTESIAN_POINT('',(100.,25.,28.2));
#13888=CARTESIAN_POINT('Origin',(100.,25.,26.5));
#13889=CARTESIAN_POINT('',(100.,-25.,68.2));
#13890=CARTESIAN_POINT('Origin',(100.,-25.,66.5));
#13891=CARTESIAN_POINT('',(100.,-25.,28.2));
#13892=CARTESIAN_POINT('Origin',(100.,-25.,26.5));
#13893=CARTESIAN_POINT('',(100.,25.,68.2));
#13894=CARTESIAN_POINT('Origin',(100.,25.,66.5));
#13895=CARTESIAN_POINT('',(100.,-7.9602041944578E-16,54.));
#13896=CARTESIAN_POINT('Origin',(100.,0.,47.5));
#13897=CARTESIAN_POINT('Origin',(102.929289321881,-25.,66.5));
#13898=CARTESIAN_POINT('',(102.858578643763,-25.,69.6085786437627));
#13899=CARTESIAN_POINT('Origin',(102.858578643763,-25.,66.5));
#13900=CARTESIAN_POINT('',(103.,-25.,69.95));
#13901=CARTESIAN_POINT('',(102.929289321881,-25.,69.7792893218814));
#13902=CARTESIAN_POINT('Origin',(103.,-25.,66.5));
#13903=CARTESIAN_POINT('Origin',(103.,0.,46.55));
#13904=CARTESIAN_POINT('',(103.,25.1,22.7));
#13905=CARTESIAN_POINT('',(103.,-25.1,22.7));
#13906=CARTESIAN_POINT('',(103.,-14.55,22.7));
#13907=CARTESIAN_POINT('',(103.,28.9,26.5));
#13908=CARTESIAN_POINT('Origin',(103.,25.1,26.5));
#13909=CARTESIAN_POINT('',(103.,28.9,66.6));
#13910=CARTESIAN_POINT('',(103.,28.9,34.525));
#13911=CARTESIAN_POINT('',(103.,25.1,70.4));
#13912=CARTESIAN_POINT('Origin',(103.,25.1,66.6));
#13913=CARTESIAN_POINT('',(103.,-25.1,70.4));
#13914=CARTESIAN_POINT('',(103.,14.55,70.4));
#13915=CARTESIAN_POINT('',(103.,-28.9,66.6));
#13916=CARTESIAN_POINT('Origin',(103.,-25.1,66.6));
#13917=CARTESIAN_POINT('',(103.,-28.9,26.5));
#13918=CARTESIAN_POINT('',(103.,-28.9,58.575));
#13919=CARTESIAN_POINT('Origin',(103.,-25.1,26.5));
#13920=CARTESIAN_POINT('',(103.,-25.,29.95));
#13921=CARTESIAN_POINT('Origin',(103.,-25.,26.5));
#13922=CARTESIAN_POINT('',(103.,-7.9602041944578E-16,54.));
#13923=CARTESIAN_POINT('Origin',(103.,0.,47.5));
#13924=CARTESIAN_POINT('',(103.,25.,69.95));
#13925=CARTESIAN_POINT('Origin',(103.,25.,66.5));
#13926=CARTESIAN_POINT('',(103.,25.,29.95));
#13927=CARTESIAN_POINT('Origin',(103.,25.,26.5));
#13928=CARTESIAN_POINT('Origin',(102.225,-25.,66.5));
#13929=CARTESIAN_POINT('',(101.45,-25.,68.2));
#13930=CARTESIAN_POINT('',(102.225,-25.,68.975));
#13931=CARTESIAN_POINT('Origin',(101.45,-25.,66.5));
#13932=CARTESIAN_POINT('Origin',(102.9,-14.55,22.6));
#13933=CARTESIAN_POINT('',(102.8,25.1,22.5));
#13934=CARTESIAN_POINT('',(102.8,25.1,22.5));
#13935=CARTESIAN_POINT('',(102.8,-25.1,22.5));
#13936=CARTESIAN_POINT('',(103.,-25.1,22.7));
#13937=CARTESIAN_POINT('',(102.8,-14.55,22.5));
#13938=CARTESIAN_POINT('Origin',(102.9,25.1,26.5));
#13939=CARTESIAN_POINT('',(102.8,29.1,26.5));
#13940=CARTESIAN_POINT('Origin',(102.8,25.1,26.5));
#13941=CARTESIAN_POINT('',(102.8,29.1,26.5));
#13942=CARTESIAN_POINT('Origin',(102.9,29.,34.525));
#13943=CARTESIAN_POINT('',(102.8,29.1,66.6));
#13944=CARTESIAN_POINT('',(102.8,29.1,34.525));
#13945=CARTESIAN_POINT('Origin',(102.9,25.1,66.6));
#13946=CARTESIAN_POINT('',(102.8,25.1,70.6));
#13947=CARTESIAN_POINT('Origin',(102.9,14.55,70.5));
#13948=CARTESIAN_POINT('',(102.8,-25.1,70.6));
#13949=CARTESIAN_POINT('Origin',(102.9,-25.1,66.6));
#13950=CARTESIAN_POINT('',(102.8,-29.1,66.6));
#13951=CARTESIAN_POINT('Origin',(102.9,-29.,58.575));
#13952=CARTESIAN_POINT('',(102.8,-29.1,26.5));
#13953=CARTESIAN_POINT('Origin',(102.9,-25.1,26.5));
#13954=CARTESIAN_POINT('Origin',(102.8,-25.1,26.5));
#13955=CARTESIAN_POINT('Origin',(100.,29.1,22.5));
#13956=CARTESIAN_POINT('',(100.,29.1,26.5));
#13957=CARTESIAN_POINT('Origin',(100.,25.1,26.5));
#13958=CARTESIAN_POINT('',(100.,25.1,22.5));
#13959=CARTESIAN_POINT('Origin',(100.,-29.1,22.5));
#13960=CARTESIAN_POINT('',(100.,-25.1,22.5));
#13961=CARTESIAN_POINT('Origin',(102.929289321881,25.,26.5));
#13962=CARTESIAN_POINT('',(102.858578643763,25.,29.6085786437627));
#13963=CARTESIAN_POINT('Origin',(102.858578643763,25.,26.5));
#13964=CARTESIAN_POINT('',(102.929289321881,25.,29.7792893218814));
#13965=CARTESIAN_POINT('Origin',(102.225,25.,26.5));
#13966=CARTESIAN_POINT('',(101.45,25.,28.2));
#13967=CARTESIAN_POINT('',(102.225,25.,28.975));
#13968=CARTESIAN_POINT('Origin',(101.45,25.,26.5));
#13969=CARTESIAN_POINT('Origin',(102.929289321881,-25.,26.5));
#13970=CARTESIAN_POINT('',(102.858578643763,-25.,29.6085786437627));
#13971=CARTESIAN_POINT('Origin',(102.858578643763,-25.,26.5));
#13972=CARTESIAN_POINT('',(102.929289321881,-25.,29.7792893218814));
#13973=CARTESIAN_POINT('Origin',(102.225,-25.,26.5));
#13974=CARTESIAN_POINT('',(101.45,-25.,28.2));
#13975=CARTESIAN_POINT('',(102.225,-25.,28.975));
#13976=CARTESIAN_POINT('Origin',(101.45,-25.,26.5));
#13977=CARTESIAN_POINT('Origin',(102.929289321881,25.,66.5));
#13978=CARTESIAN_POINT('',(102.858578643763,25.,69.6085786437627));
#13979=CARTESIAN_POINT('Origin',(102.858578643763,25.,66.5));
#13980=CARTESIAN_POINT('',(102.929289321881,25.,69.7792893218814));
#13981=CARTESIAN_POINT('Origin',(102.225,25.,66.5));
#13982=CARTESIAN_POINT('',(101.45,25.,68.2));
#13983=CARTESIAN_POINT('',(102.225,25.,68.975));
#13984=CARTESIAN_POINT('Origin',(101.45,25.,66.5));
#13985=CARTESIAN_POINT('Origin',(103.,25.,66.5));
#13986=CARTESIAN_POINT('',(103.,25.,68.2));
#13987=CARTESIAN_POINT('Origin',(103.,-25.,26.5));
#13988=CARTESIAN_POINT('',(103.,-25.,28.2));
#13989=CARTESIAN_POINT('Origin',(103.,-25.,66.5));
#13990=CARTESIAN_POINT('',(103.,-25.,68.2));
#13991=CARTESIAN_POINT('Origin',(103.,25.,26.5));
#13992=CARTESIAN_POINT('',(103.,25.,28.2));
#13993=CARTESIAN_POINT('Origin',(103.,0.,47.5));
#13994=CARTESIAN_POINT('',(103.,7.9602041944578E-16,54.));
#13995=CARTESIAN_POINT('Origin',(100.,-25.1,26.5));
#13996=CARTESIAN_POINT('',(0.,0.,0.));
#13997=CARTESIAN_POINT('Origin',(0.25,25.,66.5));
#13998=CARTESIAN_POINT('',(0.,25.,68.55));
#13999=CARTESIAN_POINT('Origin',(0.,25.,66.5));
#14000=CARTESIAN_POINT('',(0.5,25.,68.05));
#14001=CARTESIAN_POINT('',(0.25,25.,68.3));
#14002=CARTESIAN_POINT('Origin',(0.5,25.,66.5));
#14003=CARTESIAN_POINT('Origin',(0.,19.075,47.5));
#14004=CARTESIAN_POINT('',(0.,26.3437390864656,94.3366323052791));
#14005=CARTESIAN_POINT('',(0.,3.65,71.6428932188134));
#14006=CARTESIAN_POINT('',(0.,12.9723033905933,80.9651966094067));
#14007=CARTESIAN_POINT('',(0.,26.9795649469519,94.6));
#14008=CARTESIAN_POINT('',(0.,15.0605866884815,89.6629975557115));
#14009=CARTESIAN_POINT('',(0.,34.2343145750508,94.6));
#14010=CARTESIAN_POINT('',(0.,27.0375,94.6));
#14011=CARTESIAN_POINT('',(0.,34.6,94.2343145750508));
#14012=CARTESIAN_POINT('',(0.,42.3109072875254,86.5234072875254));
#14013=CARTESIAN_POINT('',(0.,34.6,73.3656854249492));
#14014=CARTESIAN_POINT('',(0.,34.6,23.75));
#14015=CARTESIAN_POINT('',(0.,34.5343145750508,73.3));
#14016=CARTESIAN_POINT('',(0.,24.2359072875254,63.0015927124745));
#14017=CARTESIAN_POINT('',(0.,34.1,73.3));
#14018=CARTESIAN_POINT('',(0.,27.5375,73.3));
#14019=CARTESIAN_POINT('',(0.,34.1,21.8));
#14020=CARTESIAN_POINT('',(0.,34.1,60.2));
#14021=CARTESIAN_POINT('',(0.,34.5343145750508,21.8));
#14022=CARTESIAN_POINT('',(0.,26.7875,21.8));
#14023=CARTESIAN_POINT('',(0.,34.6,21.7343145750508));
#14024=CARTESIAN_POINT('',(0.,24.2609072875253,32.0734072875253));
#14025=CARTESIAN_POINT('',(0.,34.6,0.765685424949272));
#14026=CARTESIAN_POINT('',(0.,34.6,23.75));
#14027=CARTESIAN_POINT('',(0.,34.2343145750507,0.399999999999999));
#14028=CARTESIAN_POINT('',(0.,42.3109072875254,8.47659271247462));
#14029=CARTESIAN_POINT('',(0.,29.1656854249492,0.4));
#14030=CARTESIAN_POINT('',(0.,23.7375,0.4));
#14031=CARTESIAN_POINT('',(0.,28.8,0.765685424949238));
#14032=CARTESIAN_POINT('',(0.,14.7765927124746,14.7890927124745));
#14033=CARTESIAN_POINT('',(0.,28.8,9.9));
#14034=CARTESIAN_POINT('',(0.,28.8,28.5));
#14035=CARTESIAN_POINT('',(0.,22.2,9.9));
#14036=CARTESIAN_POINT('',(0.,20.8375,9.9));
#14037=CARTESIAN_POINT('',(0.,22.2,4.76568542494924));
#14038=CARTESIAN_POINT('',(0.,22.2,25.9));
#14039=CARTESIAN_POINT('',(0.,22.1343145750508,4.7));
#14040=CARTESIAN_POINT('',(0.,32.0859072875254,14.6515927124747));
#14041=CARTESIAN_POINT('',(0.,13.4795649469519,4.7));
#14042=CARTESIAN_POINT('',(0.,16.0875,4.7));
#14043=CARTESIAN_POINT('',(0.,13.3558711208215,4.751235660365));
#14044=CARTESIAN_POINT('',(0.,8.21024487335069,6.88262383897043));
#14045=CARTESIAN_POINT('',(0.,3.65,14.4571067811865));
#14046=CARTESIAN_POINT('',(0.,-0.827696609406725,18.9348033905933));
#14047=CARTESIAN_POINT('',(0.,3.65,33.9841759407722));
#14048=CARTESIAN_POINT('',(0.,3.65,59.675));
#14049=CARTESIAN_POINT('',(0.,3.65,61.0158240592278));
#14050=CARTESIAN_POINT('Origin',(0.,0.,47.5));
#14051=CARTESIAN_POINT('',(0.,3.65,59.675));
#14052=CARTESIAN_POINT('',(0.,25.,28.55));
#14053=CARTESIAN_POINT('Origin',(0.,25.,26.5));
#14054=CARTESIAN_POINT('Origin',(0.,25.,66.5));
#14055=CARTESIAN_POINT('',(8.,25.,68.05));
#14056=CARTESIAN_POINT('',(0.,25.,68.05));
#14057=CARTESIAN_POINT('Origin',(8.,25.,66.5));
#14058=CARTESIAN_POINT('Origin',(0.25,25.,26.5));
#14059=CARTESIAN_POINT('',(0.5,25.,28.05));
#14060=CARTESIAN_POINT('',(0.25,25.,28.3));
#14061=CARTESIAN_POINT('Origin',(0.5,25.,26.5));
#14062=CARTESIAN_POINT('Origin',(0.,25.,26.5));
#14063=CARTESIAN_POINT('',(8.,25.,28.05));
#14064=CARTESIAN_POINT('',(0.,25.,28.05));
#14065=CARTESIAN_POINT('Origin',(8.,25.,26.5));
#14066=CARTESIAN_POINT('Origin',(0.,25.9299291191192,94.4946300940827));
#14067=CARTESIAN_POINT('',(99.6456708580913,26.1430277504891,94.6370180473338));
#14068=CARTESIAN_POINT('',(99.6,26.3376756975437,94.7670776474706));
#14069=CARTESIAN_POINT('',(98.9677437265672,29.0323346284133,96.5675911815562));
#14070=CARTESIAN_POINT('',(0.4,26.3376756975437,94.7670776474706));
#14071=CARTESIAN_POINT('',(0.,26.3376756975437,94.7670776474706));
#14072=CARTESIAN_POINT('',(0.354329141908731,26.143027750489,94.6370180473338));
#14073=CARTESIAN_POINT('',(-0.800981938914284,21.2191235478949,91.3469704439993));
#14074=CARTESIAN_POINT('',(0.5,25.5221825406948,94.2221825406948));
#14075=CARTESIAN_POINT('',(2.11739775967216,18.6288775613602,89.6162234088404));
#14076=CARTESIAN_POINT('',(99.5,25.5221825406948,94.2221825406948));
#14077=CARTESIAN_POINT('',(0.,25.5221825406948,94.2221825406948));
#14078=CARTESIAN_POINT('',(96.0493640279813,10.8156664808431,84.3956026712843));
#14079=CARTESIAN_POINT('Origin',(0.,26.387867965644,94.787867965644));
#14080=CARTESIAN_POINT('',(99.6,26.4380602337443,94.8086582838175));
#14081=CARTESIAN_POINT('',(99.6,14.9075133155355,90.032549368716));
#14082=CARTESIAN_POINT('',(0.4,26.4380602337443,94.8086582838175));
#14083=CARTESIAN_POINT('',(0.,26.4380602337443,94.8086582838175));
#14084=CARTESIAN_POINT('',(0.4,14.9075133155355,90.032549368716));
#14085=CARTESIAN_POINT('Origin',(99.8,14.9840500020085,89.8477734622137));
#14086=CARTESIAN_POINT('',(100.,26.3437390864656,94.3366323052791));
#14087=CARTESIAN_POINT('',(100.105946489469,26.4037529519037,94.2468152084245));
#14088=CARTESIAN_POINT('',(100.,26.9795649469519,94.6));
#14089=CARTESIAN_POINT('',(100.,15.0605866884815,89.6629975557115));
#14090=CARTESIAN_POINT('',(99.6956708580913,26.9190301168722,94.9043291419087));
#14091=CARTESIAN_POINT('',(100.,26.9795649469519,94.6));
#14092=CARTESIAN_POINT('',(96.6772607457411,11.7444577556222,91.8859190295585));
#14093=CARTESIAN_POINT('Origin',(99.75,12.7955266952966,81.1419733047034));
#14094=CARTESIAN_POINT('',(99.5,3.50355339059328,72.2035533905933));
#14095=CARTESIAN_POINT('',(99.5,12.61875,81.31875));
#14096=CARTESIAN_POINT('',(100.,3.65,71.6428932188134));
#14097=CARTESIAN_POINT('',(99.5,3.50355339059328,72.2035533905933));
#14098=CARTESIAN_POINT('',(100.,12.9723033905933,80.9651966094067));
#14099=CARTESIAN_POINT('Origin',(0.,26.9190301168722,94.9043291419087));
#14100=CARTESIAN_POINT('',(0.304329141908727,26.9190301168722,94.9043291419087));
#14101=CARTESIAN_POINT('',(1.48950104191211,20.9607686190275,93.7191572419054));
#14102=CARTESIAN_POINT('',(99.6,27.4,95.));
#14103=CARTESIAN_POINT('',(97.8609183745487,36.1429537356614,96.7390816254513));
#14104=CARTESIAN_POINT('',(0.4,27.4,95.));
#14105=CARTESIAN_POINT('',(0.,27.4,95.));
#14106=CARTESIAN_POINT('',(0.305843413104347,26.9266428722557,94.9058434131043));
#14107=CARTESIAN_POINT('Origin',(0.2,14.9840500020085,89.8477734622137));
#14108=CARTESIAN_POINT('',(0.,26.9795649469519,94.6));
#14109=CARTESIAN_POINT('',(-0.105946489468213,26.4037529519034,94.246815208425));
#14110=CARTESIAN_POINT('Origin',(0.2,27.0375,94.8));
#14111=CARTESIAN_POINT('',(0.4,34.4,95.));
#14112=CARTESIAN_POINT('',(0.4,27.0375,95.));
#14113=CARTESIAN_POINT('',(0.,34.2343145750508,94.6));
#14114=CARTESIAN_POINT('Origin',(99.75,25.,26.5));
#14115=CARTESIAN_POINT('',(100.,25.,28.55));
#14116=CARTESIAN_POINT('Origin',(100.,25.,26.5));
#14117=CARTESIAN_POINT('',(99.5,25.,28.05));
#14118=CARTESIAN_POINT('',(99.75,25.,28.3));
#14119=CARTESIAN_POINT('Origin',(99.5,25.,26.5));
#14120=CARTESIAN_POINT('Origin',(100.,19.075,47.5));
#14121=CARTESIAN_POINT('',(100.,3.65,61.0158240592278));
#14122=CARTESIAN_POINT('',(100.,3.65,59.675));
#14123=CARTESIAN_POINT('',(100.,3.65,33.9841759407722));
#14124=CARTESIAN_POINT('Origin',(100.,0.,47.5));
#14125=CARTESIAN_POINT('',(100.,3.65,14.4571067811865));
#14126=CARTESIAN_POINT('',(100.,3.65,59.675));
#14127=CARTESIAN_POINT('',(100.,13.3558711208215,4.751235660365));
#14128=CARTESIAN_POINT('',(100.,-0.827696609406725,18.9348033905933));
#14129=CARTESIAN_POINT('',(100.,13.4795649469519,4.7));
#14130=CARTESIAN_POINT('',(100.,8.21024487335069,6.88262383897043));
#14131=CARTESIAN_POINT('',(100.,22.1343145750508,4.7));
#14132=CARTESIAN_POINT('',(100.,16.0875,4.7));
#14133=CARTESIAN_POINT('',(100.,22.2,4.76568542494924));
#14134=CARTESIAN_POINT('',(100.,32.0859072875254,14.6515927124747));
#14135=CARTESIAN_POINT('',(100.,22.2,9.9));
#14136=CARTESIAN_POINT('',(100.,22.2,25.9));
#14137=CARTESIAN_POINT('',(100.,28.8,9.9));
#14138=CARTESIAN_POINT('',(100.,20.8375,9.9));
#14139=CARTESIAN_POINT('',(100.,28.8,0.765685424949241));
#14140=CARTESIAN_POINT('',(100.,28.8,28.5));
#14141=CARTESIAN_POINT('',(100.,29.1656854249492,0.4));
#14142=CARTESIAN_POINT('',(100.,14.7765927124746,14.7890927124745));
#14143=CARTESIAN_POINT('',(100.,34.2343145750507,0.4));
#14144=CARTESIAN_POINT('',(100.,23.7375,0.4));
#14145=CARTESIAN_POINT('',(100.,34.6,0.765685424949272));
#14146=CARTESIAN_POINT('',(100.,42.3109072875254,8.47659271247462));
#14147=CARTESIAN_POINT('',(100.,34.6,21.7343145750508));
#14148=CARTESIAN_POINT('',(100.,34.6,23.75));
#14149=CARTESIAN_POINT('',(100.,34.5343145750508,21.8));
#14150=CARTESIAN_POINT('',(100.,24.2609072875253,32.0734072875253));
#14151=CARTESIAN_POINT('',(100.,34.1,21.8));
#14152=CARTESIAN_POINT('',(100.,26.7875,21.8));
#14153=CARTESIAN_POINT('',(100.,34.1,73.3));
#14154=CARTESIAN_POINT('',(100.,34.1,60.2));
#14155=CARTESIAN_POINT('',(100.,34.5343145750508,73.3));
#14156=CARTESIAN_POINT('',(100.,27.5375,73.3));
#14157=CARTESIAN_POINT('',(100.,34.6,73.3656854249493));
#14158=CARTESIAN_POINT('',(100.,24.2359072875254,63.0015927124745));
#14159=CARTESIAN_POINT('',(100.,34.6,94.2343145750508));
#14160=CARTESIAN_POINT('',(100.,34.6,23.75));
#14161=CARTESIAN_POINT('',(100.,34.2343145750508,94.6));
#14162=CARTESIAN_POINT('',(100.,42.3109072875254,86.5234072875254));
#14163=CARTESIAN_POINT('',(100.,27.0375,94.6));
#14164=CARTESIAN_POINT('',(100.,25.,68.55));
#14165=CARTESIAN_POINT('Origin',(100.,25.,66.5));
#14166=CARTESIAN_POINT('Origin',(100.,25.,26.5));
#14167=CARTESIAN_POINT('',(92.,25.,28.05));
#14168=CARTESIAN_POINT('',(100.,25.,28.05));
#14169=CARTESIAN_POINT('Origin',(92.,25.,26.5));
#14170=CARTESIAN_POINT('Origin',(99.75,25.,66.5));
#14171=CARTESIAN_POINT('',(99.5,25.,68.05));
#14172=CARTESIAN_POINT('',(99.75,25.,68.3));
#14173=CARTESIAN_POINT('Origin',(99.5,25.,66.5));
#14174=CARTESIAN_POINT('Origin',(100.,25.,66.5));
#14175=CARTESIAN_POINT('',(92.,25.,68.05));
#14176=CARTESIAN_POINT('',(100.,25.,68.05));
#14177=CARTESIAN_POINT('Origin',(92.,25.,66.5));
#14178=CARTESIAN_POINT('Origin',(0.,3.65,71.6428932188134));
#14179=CARTESIAN_POINT('',(0.5,3.50355339059328,72.2035533905933));
#14180=CARTESIAN_POINT('',(0.5,3.15,71.35));
#14181=CARTESIAN_POINT('',(0.5,3.50355339059328,72.2035533905933));
#14182=CARTESIAN_POINT('',(0.,3.65,71.6428932188134));
#14183=CARTESIAN_POINT('',(0.5,3.15,71.35));
#14184=CARTESIAN_POINT('Origin',(0.25,12.7955266952966,81.1419733047034));
#14185=CARTESIAN_POINT('',(0.5,12.61875,81.31875));
#14186=CARTESIAN_POINT('Origin',(0.25,3.4,59.675));
#14187=CARTESIAN_POINT('',(0.5,3.15,61.1410226889336));
#14188=CARTESIAN_POINT('Origin',(3.65,0.,47.5));
#14189=CARTESIAN_POINT('',(0.5,3.15,59.675));
#14190=CARTESIAN_POINT('Origin',(99.5,3.15,71.35));
#14191=CARTESIAN_POINT('',(99.5,3.15,71.35));
#14192=CARTESIAN_POINT('',(99.5,3.15,71.35));
#14193=CARTESIAN_POINT('',(100.,3.65,71.6428932188134));
#14194=CARTESIAN_POINT('Origin',(0.,3.32677669529664,71.7767766952966));
#14195=CARTESIAN_POINT('',(0.,3.50355339059328,72.2035533905933));
#14196=CARTESIAN_POINT('',(0.,3.15,71.35));
#14197=CARTESIAN_POINT('Origin',(99.75,3.4,59.675));
#14198=CARTESIAN_POINT('',(99.5,3.15,61.1410226889336));
#14199=CARTESIAN_POINT('Origin',(96.3499999999999,0.,47.5));
#14200=CARTESIAN_POINT('',(99.5,3.15,59.675));
#14201=CARTESIAN_POINT('Origin',(0.,26.3,95.));
#14202=CARTESIAN_POINT('Origin',(0.5,3.50355339059327,13.8964466094067));
#14203=CARTESIAN_POINT('',(0.5,3.15,14.75));
#14204=CARTESIAN_POINT('',(0.,3.65,14.4571067811866));
#14205=CARTESIAN_POINT('',(0.5,3.50355339059327,13.8964466094067));
#14206=CARTESIAN_POINT('',(0.5,3.50355339059327,13.8964466094067));
#14207=CARTESIAN_POINT('',(0.5,3.15,14.75));
#14208=CARTESIAN_POINT('Origin',(0.25,-1.00447330470336,18.7580266952966));
#14209=CARTESIAN_POINT('',(0.4,13.1292893218813,4.41213203435597));
#14210=CARTESIAN_POINT('',(0.5,12.887867965644,4.51213203435597));
#14211=CARTESIAN_POINT('',(3.45785529853279,5.746973588389,7.4699873328888));
#14212=CARTESIAN_POINT('',(0.5,-1.18125,18.58125));
#14213=CARTESIAN_POINT('',(-0.48589817198775,13.6311103255984,5.16316024034552));
#14214=CARTESIAN_POINT('Origin',(99.5,3.50355339059327,13.8964466094067));
#14215=CARTESIAN_POINT('',(99.5,3.15,14.75));
#14216=CARTESIAN_POINT('',(99.5,3.15,14.75));
#14217=CARTESIAN_POINT('',(99.5,3.50355339059327,13.8964466094067));
#14218=CARTESIAN_POINT('',(99.5,3.50355339059327,13.8964466094067));
#14219=CARTESIAN_POINT('',(100.,3.65,14.4571067811865));
#14220=CARTESIAN_POINT('Origin',(0.,3.32677669529664,14.3232233047034));
#14221=CARTESIAN_POINT('',(0.,3.15,14.75));
#14222=CARTESIAN_POINT('',(0.,3.50355339059327,13.8964466094067));
#14223=CARTESIAN_POINT('Origin',(99.75,-1.00447330470336,18.7580266952966));
#14224=CARTESIAN_POINT('',(99.6,13.1292893218814,4.41213203435595));
#14225=CARTESIAN_POINT('',(100.485898171988,13.6311103255987,5.16316024034602));
#14226=CARTESIAN_POINT('',(99.5,12.887867965644,4.51213203435597));
#14227=CARTESIAN_POINT('',(99.5,-1.18125,18.58125));
#14228=CARTESIAN_POINT('',(90.1551656566029,-9.67255784431481,13.856966377753));
#14229=CARTESIAN_POINT('Origin',(99.75,3.4,59.675));
#14230=CARTESIAN_POINT('',(99.5,3.15,33.8589773110664));
#14231=CARTESIAN_POINT('Origin',(96.3499999999999,0.,47.5));
#14232=CARTESIAN_POINT('',(99.5,3.15,59.675));
#14233=CARTESIAN_POINT('Origin',(0.25,3.4,59.675));
#14234=CARTESIAN_POINT('',(0.5,3.15,33.8589773110664));
#14235=CARTESIAN_POINT('Origin',(3.65,0.,47.5));
#14236=CARTESIAN_POINT('',(0.5,3.15,59.675));
#14237=CARTESIAN_POINT('Origin',(0.,3.15,71.85));
#14238=CARTESIAN_POINT('',(0.,3.15,33.8589773110664));
#14239=CARTESIAN_POINT('',(77.5,3.15,19.));
#14240=CARTESIAN_POINT('Origin',(80.,3.15,19.));
#14241=CARTESIAN_POINT('',(47.5,3.15,19.));
#14242=CARTESIAN_POINT('Origin',(50.,3.15,19.));
#14243=CARTESIAN_POINT('',(17.5,3.15,19.));
#14244=CARTESIAN_POINT('Origin',(20.,3.15,19.));
#14245=CARTESIAN_POINT('Origin',(0.,0.,47.5));
#14246=CARTESIAN_POINT('',(0.,3.15,61.1410226889336));
#14247=CARTESIAN_POINT('Origin',(99.8,8.13370818687767,6.69784793246817));
#14248=CARTESIAN_POINT('',(99.6,13.4,4.3));
#14249=CARTESIAN_POINT('',(99.6,8.05717150040465,6.51307202596591));
#14250=CARTESIAN_POINT('',(100.,13.4795649469519,4.7));
#14251=CARTESIAN_POINT('Origin',(99.8,26.7875,22.));
#14252=CARTESIAN_POINT('',(99.6,34.7,22.2));
#14253=CARTESIAN_POINT('',(99.6,34.5,22.2));
#14254=CARTESIAN_POINT('',(99.6,26.7875,22.2));
#14255=CARTESIAN_POINT('',(99.6,34.5,22.2));
#14256=CARTESIAN_POINT('',(100.,34.5343145750508,21.8));
#14257=CARTESIAN_POINT('Origin',(99.8,27.0375,94.8));
#14258=CARTESIAN_POINT('',(99.6,34.4,95.));
#14259=CARTESIAN_POINT('',(100.,34.2343145750508,94.6));
#14260=CARTESIAN_POINT('',(99.6,27.0375,95.));
#14261=CARTESIAN_POINT('Origin',(99.8,42.4523286437627,86.6648286437627));
#14262=CARTESIAN_POINT('',(99.6,35.,94.4));
#14263=CARTESIAN_POINT('',(100.,34.6,94.2343145750508));
#14264=CARTESIAN_POINT('',(99.6,42.59375,86.80625));
#14265=CARTESIAN_POINT('Origin',(99.8,34.8,23.75));
#14266=CARTESIAN_POINT('',(99.6,35.,73.2));
#14267=CARTESIAN_POINT('',(100.,34.6,73.3656854249493));
#14268=CARTESIAN_POINT('',(99.6,35.,23.75));
#14269=CARTESIAN_POINT('Origin',(99.8,24.3773286437628,62.8601713562372));
#14270=CARTESIAN_POINT('',(99.6,34.7,72.9));
#14271=CARTESIAN_POINT('',(99.6,24.5187500000001,62.7187499999999));
#14272=CARTESIAN_POINT('',(100.,34.5343145750508,73.3));
#14273=CARTESIAN_POINT('Origin',(99.8,27.5375,73.1));
#14274=CARTESIAN_POINT('',(99.6,34.5,72.9));
#14275=CARTESIAN_POINT('',(99.6,27.5375,72.9));
#14276=CARTESIAN_POINT('',(100.,34.1,73.3));
#14277=CARTESIAN_POINT('Origin',(99.8,34.3,60.2));
#14278=CARTESIAN_POINT('',(99.6,34.5,60.2));
#14279=CARTESIAN_POINT('Origin',(99.8,24.4023286437626,32.2148286437626));
#14280=CARTESIAN_POINT('',(99.6,35.,21.9));
#14281=CARTESIAN_POINT('',(99.6,24.5437499999999,32.3562499999999));
#14282=CARTESIAN_POINT('',(100.,34.6,21.7343145750508));
#14283=CARTESIAN_POINT('Origin',(99.8,34.8,23.75));
#14284=CARTESIAN_POINT('',(99.6,35.,0.6));
#14285=CARTESIAN_POINT('',(99.6,35.,23.75));
#14286=CARTESIAN_POINT('',(100.,34.6,0.765685424949275));
#14287=CARTESIAN_POINT('Origin',(99.8,42.4523286437627,8.33517135623731));
#14288=CARTESIAN_POINT('',(99.6,34.4,0.));
#14289=CARTESIAN_POINT('',(99.6,42.59375,8.19374999999999));
#14290=CARTESIAN_POINT('',(100.,34.2343145750507,0.4));
#14291=CARTESIAN_POINT('Origin',(99.8,23.7375,0.2));
#14292=CARTESIAN_POINT('',(99.6,29.,0.));
#14293=CARTESIAN_POINT('',(99.6,23.7375,0.));
#14294=CARTESIAN_POINT('',(100.,29.1656854249492,0.4));
#14295=CARTESIAN_POINT('Origin',(99.8,14.6351713562373,14.6476713562372));
#14296=CARTESIAN_POINT('',(99.6,28.4,0.6));
#14297=CARTESIAN_POINT('',(99.6,14.49375,14.5062499999999));
#14298=CARTESIAN_POINT('',(100.,28.8,0.765685424949241));
#14299=CARTESIAN_POINT('Origin',(99.8,28.6,28.5));
#14300=CARTESIAN_POINT('',(99.6,28.4,9.5));
#14301=CARTESIAN_POINT('',(99.6,28.4,28.5));
#14302=CARTESIAN_POINT('',(100.,28.8,9.9));
#14303=CARTESIAN_POINT('Origin',(99.8,20.8375,9.7));
#14304=CARTESIAN_POINT('',(99.6,22.6,9.5));
#14305=CARTESIAN_POINT('',(99.6,20.8375,9.5));
#14306=CARTESIAN_POINT('',(100.,22.2,9.9));
#14307=CARTESIAN_POINT('Origin',(99.8,22.4,25.9));
#14308=CARTESIAN_POINT('',(99.6,22.6,4.6));
#14309=CARTESIAN_POINT('',(99.6,22.6,25.9));
#14310=CARTESIAN_POINT('',(100.,22.2,4.76568542494924));
#14311=CARTESIAN_POINT('Origin',(99.8,32.2273286437627,14.5101713562374));
#14312=CARTESIAN_POINT('',(99.6,22.3,4.3));
#14313=CARTESIAN_POINT('',(99.6,32.36875,14.3687500000001));
#14314=CARTESIAN_POINT('',(100.,22.1343145750508,4.7));
#14315=CARTESIAN_POINT('Origin',(99.8,16.0875,4.5));
#14316=CARTESIAN_POINT('',(99.6,16.0875,4.3));
#14317=CARTESIAN_POINT('Origin',(0.,28.7,0.3));
#14318=CARTESIAN_POINT('',(0.4,28.4,0.6));
#14319=CARTESIAN_POINT('',(0.,28.4,0.6));
#14320=CARTESIAN_POINT('',(0.4,29.,0.));
#14321=CARTESIAN_POINT('',(0.4,14.49375,14.5062499999999));
#14322=CARTESIAN_POINT('',(0.,29.,0.));
#14323=CARTESIAN_POINT('Origin',(0.,28.4,9.5));
#14324=CARTESIAN_POINT('',(0.4,28.4,9.5));
#14325=CARTESIAN_POINT('',(0.,28.4,9.5));
#14326=CARTESIAN_POINT('',(0.4,28.4,28.5));
#14327=CARTESIAN_POINT('Origin',(0.,22.6,9.5));
#14328=CARTESIAN_POINT('',(0.4,22.6,9.5));
#14329=CARTESIAN_POINT('',(0.,22.6,9.5));
#14330=CARTESIAN_POINT('',(0.4,20.8375,9.5));
#14331=CARTESIAN_POINT('Origin',(0.,22.6,4.3));
#14332=CARTESIAN_POINT('',(0.4,22.6,4.6));
#14333=CARTESIAN_POINT('',(0.,22.6,4.6));
#14334=CARTESIAN_POINT('',(0.4,22.6,25.9));
#14335=CARTESIAN_POINT('Origin',(0.,22.45,4.45));
#14336=CARTESIAN_POINT('',(0.4,22.3,4.3));
#14337=CARTESIAN_POINT('',(0.,22.3,4.3));
#14338=CARTESIAN_POINT('',(0.4,32.36875,14.3687500000001));
#14339=CARTESIAN_POINT('Origin',(0.,13.1,4.3));
#14340=CARTESIAN_POINT('',(0.4,13.4,4.3));
#14341=CARTESIAN_POINT('',(0.,13.4,4.3));
#14342=CARTESIAN_POINT('',(0.4,16.0875,4.3));
#14343=CARTESIAN_POINT('Origin',(0.,13.143933982822,4.40606601717798));
#14344=CARTESIAN_POINT('',(0.4,8.05717150040465,6.51307202596591));
#14345=CARTESIAN_POINT('',(0.,12.887867965644,4.51213203435597));
#14346=CARTESIAN_POINT('Origin',(0.,3.15,14.25));
#14347=CARTESIAN_POINT('Origin',(0.2,8.13370818687767,6.69784793246817));
#14348=CARTESIAN_POINT('',(0.,13.4795649469519,4.7));
#14349=CARTESIAN_POINT('Origin',(0.2,16.0875,4.5));
#14350=CARTESIAN_POINT('',(0.,22.1343145750508,4.7));
#14351=CARTESIAN_POINT('Origin',(0.2,32.2273286437627,14.5101713562374));
#14352=CARTESIAN_POINT('',(0.,22.2,4.76568542494924));
#14353=CARTESIAN_POINT('Origin',(0.2,22.4,25.9));
#14354=CARTESIAN_POINT('',(0.,22.2,9.9));
#14355=CARTESIAN_POINT('Origin',(0.2,20.8375,9.7));
#14356=CARTESIAN_POINT('',(0.,28.8,9.9));
#14357=CARTESIAN_POINT('Origin',(0.2,28.6,28.5));
#14358=CARTESIAN_POINT('',(0.,28.8,0.765685424949238));
#14359=CARTESIAN_POINT('Origin',(0.2,14.6351713562373,14.6476713562372));
#14360=CARTESIAN_POINT('',(0.,29.1656854249492,0.4));
#14361=CARTESIAN_POINT('Origin',(0.2,23.7375,0.2));
#14362=CARTESIAN_POINT('',(0.4,34.4,0.));
#14363=CARTESIAN_POINT('',(0.,34.2343145750507,0.400000000000001));
#14364=CARTESIAN_POINT('',(0.4,23.7375,0.));
#14365=CARTESIAN_POINT('Origin',(0.2,42.4523286437627,8.33517135623731));
#14366=CARTESIAN_POINT('',(0.4,35.,0.6));
#14367=CARTESIAN_POINT('',(0.,34.6,0.765685424949272));
#14368=CARTESIAN_POINT('',(0.4,42.59375,8.19374999999999));
#14369=CARTESIAN_POINT('Origin',(0.2,34.8,23.75));
#14370=CARTESIAN_POINT('',(0.4,35.,21.9));
#14371=CARTESIAN_POINT('',(0.,34.6,21.7343145750508));
#14372=CARTESIAN_POINT('',(0.4,35.,23.75));
#14373=CARTESIAN_POINT('Origin',(0.2,24.4023286437626,32.2148286437626));
#14374=CARTESIAN_POINT('',(0.4,34.7,22.2));
#14375=CARTESIAN_POINT('',(0.,34.5343145750508,21.8));
#14376=CARTESIAN_POINT('',(0.4,24.5437499999999,32.3562499999999));
#14377=CARTESIAN_POINT('Origin',(0.2,26.7875,22.));
#14378=CARTESIAN_POINT('',(0.4,34.5,22.2));
#14379=CARTESIAN_POINT('',(0.,34.1,21.8));
#14380=CARTESIAN_POINT('',(0.4,26.7875,22.2));
#14381=CARTESIAN_POINT('Origin',(0.2,27.5375,73.1));
#14382=CARTESIAN_POINT('',(0.4,34.7,72.9));
#14383=CARTESIAN_POINT('',(0.,34.5343145750508,73.3));
#14384=CARTESIAN_POINT('',(0.4,34.5,72.9));
#14385=CARTESIAN_POINT('',(0.4,27.5375,72.9));
#14386=CARTESIAN_POINT('',(0.4,34.5,72.9));
#14387=CARTESIAN_POINT('Origin',(0.2,24.3773286437628,62.8601713562372));
#14388=CARTESIAN_POINT('',(0.4,35.,73.2));
#14389=CARTESIAN_POINT('',(0.4,24.5187500000001,62.7187499999999));
#14390=CARTESIAN_POINT('',(0.,34.6,73.3656854249492));
#14391=CARTESIAN_POINT('Origin',(0.2,34.8,23.75));
#14392=CARTESIAN_POINT('',(0.4,35.,94.4));
#14393=CARTESIAN_POINT('',(0.4,35.,23.75));
#14394=CARTESIAN_POINT('',(0.,34.6,94.2343145750508));
#14395=CARTESIAN_POINT('Origin',(0.2,34.3,60.2));
#14396=CARTESIAN_POINT('',(0.4,34.5,60.2));
#14397=CARTESIAN_POINT('Origin',(0.2,42.4523286437627,86.6648286437627));
#14398=CARTESIAN_POINT('',(0.4,42.59375,86.80625));
#14399=CARTESIAN_POINT('Origin',(0.,28.4,0.));
#14400=CARTESIAN_POINT('',(0.,34.4,0.));
#14401=CARTESIAN_POINT('Origin',(0.,34.7,0.3));
#14402=CARTESIAN_POINT('',(0.,35.,0.6));
#14403=CARTESIAN_POINT('Origin',(0.,35.,0.));
#14404=CARTESIAN_POINT('',(0.,35.,21.9));
#14405=CARTESIAN_POINT('',(17.5,35.,19.));
#14406=CARTESIAN_POINT('Origin',(20.,35.,19.));
#14407=CARTESIAN_POINT('',(47.5,35.,19.));
#14408=CARTESIAN_POINT('Origin',(50.,35.,19.));
#14409=CARTESIAN_POINT('',(77.5,35.,19.));
#14410=CARTESIAN_POINT('Origin',(80.,35.,19.));
#14411=CARTESIAN_POINT('Origin',(0.,34.85,22.05));
#14412=CARTESIAN_POINT('',(0.,34.7,22.2));
#14413=CARTESIAN_POINT('Origin',(0.,34.5,22.2));
#14414=CARTESIAN_POINT('',(0.,34.5,22.2));
#14415=CARTESIAN_POINT('Origin',(0.,34.5,72.9));
#14416=CARTESIAN_POINT('',(0.,34.5,72.9));
#14417=CARTESIAN_POINT('Origin',(0.,36.,72.9));
#14418=CARTESIAN_POINT('',(0.,34.7,72.9));
#14419=CARTESIAN_POINT('Origin',(0.,34.85,73.05));
#14420=CARTESIAN_POINT('',(0.,35.,73.2));
#14421=CARTESIAN_POINT('Origin',(0.,35.,0.));
#14422=CARTESIAN_POINT('',(0.,35.,94.4));
#14423=CARTESIAN_POINT('Origin',(0.,34.7,94.7));
#14424=CARTESIAN_POINT('',(0.,34.4,95.));
#14425=CARTESIAN_POINT('Origin',(0.,35.,95.));
#14426=CARTESIAN_POINT('Origin',(92.,25.,26.5));
#14427=CARTESIAN_POINT('Origin',(92.,25.,66.5));
#14428=CARTESIAN_POINT('Origin',(8.,25.,26.5));
#14429=CARTESIAN_POINT('Origin',(8.,25.,66.5));
#14430=CARTESIAN_POINT('Origin',(20.,35.,19.));
#14431=CARTESIAN_POINT('',(17.5,35.,19.));
#14432=CARTESIAN_POINT('Origin',(50.,35.,19.));
#14433=CARTESIAN_POINT('',(47.5,35.,19.));
#14434=CARTESIAN_POINT('Origin',(80.,35.,19.));
#14435=CARTESIAN_POINT('',(77.5,35.,19.));
#14436=CARTESIAN_POINT('Origin',(0.,3.15,71.85));
#14437=CARTESIAN_POINT('',(0.,0.,0.));
#14438=CARTESIAN_POINT('Origin',(0.,13.4,0.));
#14439=CARTESIAN_POINT('',(9.0205620750794E-16,-13.4,-1.64102671085745E-15));
#14440=CARTESIAN_POINT('Origin',(0.,0.,0.));
#14441=CARTESIAN_POINT('Origin',(0.250000000000004,0.,0.));
#14442=CARTESIAN_POINT('',(0.500000000000005,-13.9,-1.70225905081482E-15));
#14443=CARTESIAN_POINT('Origin',(0.500000000000007,0.,0.));
#14444=CARTESIAN_POINT('',(0.250000000000004,-13.65,-1.67164288083614E-15));
#14445=CARTESIAN_POINT('Origin',(43.8,0.,0.));
#14446=CARTESIAN_POINT('',(87.1,-13.9,-1.70225905081482E-15));
#14447=CARTESIAN_POINT('Origin',(87.1,0.,0.));
#14448=CARTESIAN_POINT('',(43.8,-13.9,-1.70225905081482E-15));
#14449=CARTESIAN_POINT('Origin',(87.35,0.,0.));
#14450=CARTESIAN_POINT('',(87.6,-13.4,-1.64102671085745E-15));
#14451=CARTESIAN_POINT('Origin',(87.6,0.,0.));
#14452=CARTESIAN_POINT('',(87.35,-13.65,-1.67164288083614E-15));
#14453=CARTESIAN_POINT('Origin',(87.6,0.,0.));
#14454=CARTESIAN_POINT('',(0.,0.,0.));
#14455=CARTESIAN_POINT('Origin',(-0.25,0.,0.));
#14456=CARTESIAN_POINT('',(0.,13.4,-1.64102671085745E-15));
#14457=CARTESIAN_POINT('Origin',(0.,0.,0.));
#14458=CARTESIAN_POINT('',(-0.5,13.9,1.70225905081482E-15));
#14459=CARTESIAN_POINT('',(-0.25,13.65,1.67164288083614E-15));
#14460=CARTESIAN_POINT('',(-0.5,-13.9,-1.70225905081482E-15));
#14461=CARTESIAN_POINT('Origin',(-0.5,0.,0.));
#14462=CARTESIAN_POINT('Origin',(-0.5,0.,0.));
#14463=CARTESIAN_POINT('Origin',(-2.75,0.,0.));
#14464=CARTESIAN_POINT('',(-5.5,-13.9,-1.70225905081482E-15));
#14465=CARTESIAN_POINT('',(-2.75,-13.9,-1.70225905081482E-15));
#14466=CARTESIAN_POINT('Origin',(-5.5,0.,0.));
#14467=CARTESIAN_POINT('Origin',(0.,0.,0.));
#14468=CARTESIAN_POINT('Origin',(-20.15,-0.75,3.75));
#14469=CARTESIAN_POINT('',(-19.9,3.,4.));
#14470=CARTESIAN_POINT('',(-20.4,2.82842712474619,3.5));
#14471=CARTESIAN_POINT('Ctrl Pts',(-19.9,2.99999999999999,4.00000000000001));
#14472=CARTESIAN_POINT('Ctrl Pts',(-20.157359312881,2.914213562373,3.74264068711902));
#14473=CARTESIAN_POINT('Ctrl Pts',(-20.4,2.82842712474619,3.5));
#14474=CARTESIAN_POINT('',(-20.4,-2.82842712474619,3.5));
#14475=CARTESIAN_POINT('',(-20.4,-0.75,3.5));
#14476=CARTESIAN_POINT('',(-19.9,-3.,4.));
#14477=CARTESIAN_POINT('Ctrl Pts',(-20.4,-2.82842712474619,3.5));
#14478=CARTESIAN_POINT('Ctrl Pts',(-20.157359312881,-2.914213562373,3.74264068711902));
#14479=CARTESIAN_POINT('Ctrl Pts',(-19.9,-2.99999999999999,4.00000000000001));
#14480=CARTESIAN_POINT('',(-19.9,-0.75,4.));
#14481=CARTESIAN_POINT('Origin',(-20.15,0.,0.));
#14482=CARTESIAN_POINT('Origin',(-20.4,0.,0.));
#14483=CARTESIAN_POINT('',(-19.9,-5.,-6.12323399573677E-16));
#14484=CARTESIAN_POINT('Origin',(-19.9,0.,0.));
#14485=CARTESIAN_POINT('Origin',(-19.9,0.,0.));
#14486=CARTESIAN_POINT('Origin',(-20.4,4.5,0.));
#14487=CARTESIAN_POINT('Origin',(-11.4,0.,5.));
#14488=CARTESIAN_POINT('',(-11.4,3.,4.));
#14489=CARTESIAN_POINT('',(-11.4,-3.,4.));
#14490=CARTESIAN_POINT('Origin',(-11.4,0.,0.));
#14491=CARTESIAN_POINT('',(-11.4,-6.,4.));
#14492=CARTESIAN_POINT('Origin',(-20.4,-6.,4.));
#14493=CARTESIAN_POINT('',(-12.95,-3.,4.));
#14494=CARTESIAN_POINT('',(-12.95,3.,4.));
#14495=CARTESIAN_POINT('Origin',(-12.95,0.,0.));
#14496=CARTESIAN_POINT('',(-6.,-5.,-6.12323399573677E-16));
#14497=CARTESIAN_POINT('Origin',(-6.,0.,0.));
#14498=CARTESIAN_POINT('',(-12.95,-5.,-6.12323399573677E-16));
#14499=CARTESIAN_POINT('Origin',(-6.,13.4,0.));
#14500=CARTESIAN_POINT('',(-6.,-13.4,-1.64102671085745E-15));
#14501=CARTESIAN_POINT('Origin',(-6.,0.,0.));
#14502=CARTESIAN_POINT('Origin',(-5.75,0.,0.));
#14503=CARTESIAN_POINT('',(-5.75,-13.65,-1.67164288083614E-15));
#14504=CARTESIAN_POINT('',(0.,0.,0.));
#14505=CARTESIAN_POINT('Origin',(0.175,0.,0.));
#14506=CARTESIAN_POINT('',(0.35,13.9,-1.70225905081482E-15));
#14507=CARTESIAN_POINT('',(0.35,-13.9,-1.70225905081482E-15));
#14508=CARTESIAN_POINT('Origin',(0.35,0.,0.));
#14509=CARTESIAN_POINT('Origin',(0.35,0.,0.));
#14510=CARTESIAN_POINT('',(0.,13.55,1.65939641284466E-15));
#14511=CARTESIAN_POINT('',(0.175,13.725,1.68082773182974E-15));
#14512=CARTESIAN_POINT('Origin',(0.,0.,0.));
#14513=CARTESIAN_POINT('Origin',(0.,13.9,0.));
#14514=CARTESIAN_POINT('Origin',(2.75,0.,0.));
#14515=CARTESIAN_POINT('',(5.5,-13.9,-1.70225905081482E-15));
#14516=CARTESIAN_POINT('Origin',(5.5,0.,0.));
#14517=CARTESIAN_POINT('',(2.75,-13.9,-1.70225905081482E-15));
#14518=CARTESIAN_POINT('Origin',(5.75,0.,0.));
#14519=CARTESIAN_POINT('',(6.,-13.4,-1.64102671085745E-15));
#14520=CARTESIAN_POINT('Origin',(6.,0.,0.));
#14521=CARTESIAN_POINT('',(5.75,-13.65,-1.67164288083614E-15));
#14522=CARTESIAN_POINT('Origin',(6.,5.,0.));
#14523=CARTESIAN_POINT('',(6.,-5.,-6.12323399573677E-16));
#14524=CARTESIAN_POINT('Origin',(6.,0.,0.));
#14525=CARTESIAN_POINT('Origin',(7.1,0.,0.));
#14526=CARTESIAN_POINT('',(8.2,-5.,-6.12323399573677E-16));
#14527=CARTESIAN_POINT('Origin',(8.2,0.,0.));
#14528=CARTESIAN_POINT('',(7.1,-5.,-6.12323399573677E-16));
#14529=CARTESIAN_POINT('Origin',(8.45,0.,0.));
#14530=CARTESIAN_POINT('',(8.7,-4.5,-5.51091059616309E-16));
#14531=CARTESIAN_POINT('Origin',(8.7,0.,0.));
#14532=CARTESIAN_POINT('',(8.45,-4.75,-5.81707229594993E-16));
#14533=CARTESIAN_POINT('Origin',(8.7,0.,0.));
#14534=CARTESIAN_POINT('',(0.,0.,0.));
#14535=CARTESIAN_POINT('Origin',(-0.85,0.,0.));
#14536=CARTESIAN_POINT('',(-0.7,8.5,-1.04094977927525E-15));
#14537=CARTESIAN_POINT('',(-0.7,-8.5,-1.04094977927525E-15));
#14538=CARTESIAN_POINT('Origin',(-0.7,0.,0.));
#14539=CARTESIAN_POINT('Origin',(-0.7,0.,0.));
#14540=CARTESIAN_POINT('',(-1.,8.2,1.00421037530083E-15));
#14541=CARTESIAN_POINT('',(-0.85,8.35,1.02258007728804E-15));
#14542=CARTESIAN_POINT('Origin',(-1.,0.,0.));
#14543=CARTESIAN_POINT('Origin',(-1.,8.5,0.));
#14544=CARTESIAN_POINT('',(-1.,-5.025,-6.15385016571545E-16));
#14545=CARTESIAN_POINT('Origin',(-1.,0.,0.));
#14546=CARTESIAN_POINT('Origin',(-0.5,0.,0.));
#14547=CARTESIAN_POINT('',(0.,-8.5,-1.04094977927525E-15));
#14548=CARTESIAN_POINT('Origin',(0.,0.,0.));
#14549=CARTESIAN_POINT('',(-0.5,-8.5,-1.04094977927525E-15));
#14550=CARTESIAN_POINT('Origin',(1.,0.,0.));
#14551=CARTESIAN_POINT('',(3.,-5.025,-6.15385016571545E-16));
#14552=CARTESIAN_POINT('Origin',(3.,0.,0.));
#14553=CARTESIAN_POINT('',(1.,-5.025,-6.15385016571545E-16));
#14554=CARTESIAN_POINT('Origin',(0.,6.5,0.));
#14555=CARTESIAN_POINT('',(0.,-6.5,-7.9602041944578E-16));
#14556=CARTESIAN_POINT('Origin',(0.,0.,0.));
#14557=CARTESIAN_POINT('Origin',(1.5,0.,0.));
#14558=CARTESIAN_POINT('',(3.,-6.5,-7.9602041944578E-16));
#14559=CARTESIAN_POINT('Origin',(3.,0.,0.));
#14560=CARTESIAN_POINT('',(1.5,-6.5,-7.9602041944578E-16));
#14561=CARTESIAN_POINT('Origin',(3.,5.025,0.));
#14562=CARTESIAN_POINT('',(0.,0.,0.));
#14563=CARTESIAN_POINT('Origin',(7.25,4.,-14.));
#14564=CARTESIAN_POINT('',(7.,7.5,-14.));
#14565=CARTESIAN_POINT('',(7.5,8.,-14.));
#14566=CARTESIAN_POINT('',(7.25000000000001,7.75000000000001,-14.));
#14567=CARTESIAN_POINT('',(7.5,4.,-18.));
#14568=CARTESIAN_POINT('Origin',(7.5,4.,-14.));
#14569=CARTESIAN_POINT('',(7.,4.,-17.5));
#14570=CARTESIAN_POINT('',(7.25,4.,-17.75));
#14571=CARTESIAN_POINT('Origin',(7.,4.,-14.));
#14572=CARTESIAN_POINT('Origin',(7.25,7.75,-9.));
#14573=CARTESIAN_POINT('',(7.,7.5,-6.61437827766148));
#14574=CARTESIAN_POINT('',(7.,7.5,-9.));
#14575=CARTESIAN_POINT('',(7.5,8.,-6.));
#14576=CARTESIAN_POINT('Origin',(-0.5,0.,0.));
#14577=CARTESIAN_POINT('',(7.5,8.,-9.));
#14578=CARTESIAN_POINT('Origin',(7.,0.,0.));
#14579=CARTESIAN_POINT('',(7.,-4.,-17.5));
#14580=CARTESIAN_POINT('',(7.,-4.,-17.5));
#14581=CARTESIAN_POINT('',(7.,-7.5,-14.));
#14582=CARTESIAN_POINT('Origin',(7.,-4.,-14.));
#14583=CARTESIAN_POINT('',(7.,-7.5,-6.61437827766148));
#14584=CARTESIAN_POINT('',(7.,-7.5,9.));
#14585=CARTESIAN_POINT('Origin',(7.,0.,0.));
#14586=CARTESIAN_POINT('Origin',(7.25,-4.,-14.));
#14587=CARTESIAN_POINT('',(7.5,-4.,-18.));
#14588=CARTESIAN_POINT('',(7.25,-4.,-17.75));
#14589=CARTESIAN_POINT('',(7.5,-8.,-14.));
#14590=CARTESIAN_POINT('Origin',(7.5,-4.,-14.));
#14591=CARTESIAN_POINT('',(7.25000000000001,-7.75000000000001,-14.));
#14592=CARTESIAN_POINT('Origin',(7.25,-4.,-17.75));
#14593=CARTESIAN_POINT('',(7.5,-4.,-18.));
#14594=CARTESIAN_POINT('Origin',(7.25,4.,14.));
#14595=CARTESIAN_POINT('',(7.,4.,17.5));
#14596=CARTESIAN_POINT('',(7.5,4.,18.));
#14597=CARTESIAN_POINT('',(7.25,4.,17.75));
#14598=CARTESIAN_POINT('',(7.5,8.,14.));
#14599=CARTESIAN_POINT('Origin',(7.5,4.,14.));
#14600=CARTESIAN_POINT('',(7.,7.5,14.));
#14601=CARTESIAN_POINT('',(7.25000000000001,7.75000000000001,14.));
#14602=CARTESIAN_POINT('Origin',(7.,4.,14.));
#14603=CARTESIAN_POINT('Origin',(7.25,4.,17.75));
#14604=CARTESIAN_POINT('',(7.,-4.,17.5));
#14605=CARTESIAN_POINT('',(7.,4.,17.5));
#14606=CARTESIAN_POINT('',(7.5,-4.,18.));
#14607=CARTESIAN_POINT('',(7.25,-4.,17.75));
#14608=CARTESIAN_POINT('',(7.5,4.,18.));
#14609=CARTESIAN_POINT('Origin',(7.,0.,0.));
#14610=CARTESIAN_POINT('',(7.,7.5,6.61437827766148));
#14611=CARTESIAN_POINT('',(7.,7.5,-9.));
#14612=CARTESIAN_POINT('',(7.,-7.5,6.61437827766148));
#14613=CARTESIAN_POINT('Origin',(7.,0.,0.));
#14614=CARTESIAN_POINT('',(7.,-7.5,14.));
#14615=CARTESIAN_POINT('',(7.,-7.5,9.));
#14616=CARTESIAN_POINT('Origin',(7.,-4.,14.));
#14617=CARTESIAN_POINT('Origin',(7.25,-4.,14.));
#14618=CARTESIAN_POINT('',(7.5,-8.,14.));
#14619=CARTESIAN_POINT('',(7.25000000000001,-7.75000000000001,14.));
#14620=CARTESIAN_POINT('Origin',(7.5,-4.,14.));
#14621=CARTESIAN_POINT('Origin',(7.25,-7.75,9.));
#14622=CARTESIAN_POINT('',(7.5,-8.,6.));
#14623=CARTESIAN_POINT('Origin',(-0.5,0.,0.));
#14624=CARTESIAN_POINT('',(7.5,-8.,9.));
#14625=CARTESIAN_POINT('Ctrl Pts',(0.95,1.17961196366423E-15,10.));
#14626=CARTESIAN_POINT('Ctrl Pts',(0.95,0.367045949756984,10.));
#14627=CARTESIAN_POINT('Ctrl Pts',(1.07752221450547,0.958324928147939,9.96511377603409));
#14628=CARTESIAN_POINT('Ctrl Pts',(1.50018713245098,1.6077683923816,9.87296307206958));
#14629=CARTESIAN_POINT('Ctrl Pts',(2.00962207364082,2.12638731453228,9.77676926762088));
#14630=CARTESIAN_POINT('Ctrl Pts',(2.93165725867213,2.56177645189286,9.6669255238723));
#14631=CARTESIAN_POINT('Ctrl Pts',(4.07030731706242,2.56318534961883,9.66664213097688));
#14632=CARTESIAN_POINT('Ctrl Pts',(4.98889535650575,2.12294159641258,9.77704450831748));
#14633=CARTESIAN_POINT('Ctrl Pts',(5.50075461569863,1.60769038329482,9.87315468661203));
#14634=CARTESIAN_POINT('Ctrl Pts',(5.92245203441391,0.948791196013554,9.9652950909916));
#14635=CARTESIAN_POINT('Ctrl Pts',(6.13498948573698,0.000273363131113907,
10.0233350886136));
#14636=CARTESIAN_POINT('Ctrl Pts',(5.92374215247507,-0.948040993147089,
9.96567245159996));
#14637=CARTESIAN_POINT('Ctrl Pts',(5.50129034980703,-1.60849172826648,9.87310398731735));
#14638=CARTESIAN_POINT('Ctrl Pts',(4.98823862135932,-2.12213585510122,9.7772258322794));
#14639=CARTESIAN_POINT('Ctrl Pts',(4.07315732767968,-2.56249026452942,9.66671893539352));
#14640=CARTESIAN_POINT('Ctrl Pts',(2.9258047487256,-2.55834406499343,9.66768970154396));
#14641=CARTESIAN_POINT('Ctrl Pts',(1.83672560681065,-2.04463419124632,9.79709054793077));
#14642=CARTESIAN_POINT('Ctrl Pts',(1.13859324782988,-1.16157795697479,9.95148672121565));
#14643=CARTESIAN_POINT('Ctrl Pts',(0.95,-0.367045949756973,10.));
#14644=CARTESIAN_POINT('Ctrl Pts',(0.950000000000001,-1.38777878078145E-16,
10.));
#14645=CARTESIAN_POINT('Ctrl Pts',(1.11666666666667,1.01770443923973E-15,
9.83333333333333));
#14646=CARTESIAN_POINT('Ctrl Pts',(1.11666666666667,0.338138082472203,9.83333333333333));
#14647=CARTESIAN_POINT('Ctrl Pts',(1.23189350754937,0.883178863551863,9.8030072278146));
#14648=CARTESIAN_POINT('Ctrl Pts',(1.62057462760155,1.4901917624257,9.72207568761741));
#14649=CARTESIAN_POINT('Ctrl Pts',(2.09306265257346,1.97974585787698,9.63710887331226));
#14650=CARTESIAN_POINT('Ctrl Pts',(2.96023499641486,2.39843888983004,9.53916716959576));
#14651=CARTESIAN_POINT('Ctrl Pts',(4.04169526814198,2.39979178983521,9.53891552839485));
#14652=CARTESIAN_POINT('Ctrl Pts',(4.90551921769836,1.97654795671124,9.6373419470974));
#14653=CARTESIAN_POINT('Ctrl Pts',(5.38030345361575,1.49011205526117,9.72224154959068));
#14654=CARTESIAN_POINT('Ctrl Pts',(5.76806824424246,0.874302676860821,9.80316241770464));
#14655=CARTESIAN_POINT('Ctrl Pts',(5.96009674079537,0.000236925558889436,
9.85361606443947));
#14656=CARTESIAN_POINT('Ctrl Pts',(5.76921977722431,-0.873560253900129,
9.80348804810433));
#14657=CARTESIAN_POINT('Ctrl Pts',(5.38079732434218,-1.49086268741372,9.72219615790121));
#14658=CARTESIAN_POINT('Ctrl Pts',(4.90485970439378,-1.97578737659674,9.63749666133857));
#14659=CARTESIAN_POINT('Ctrl Pts',(4.04423514273,-2.39913671465528,9.53898427715599));
#14660=CARTESIAN_POINT('Ctrl Pts',(2.95484400730983,-2.39524695639726,9.53982373563105));
#14661=CARTESIAN_POINT('Ctrl Pts',(1.93019347129584,-1.90102207176844,9.65527052164018));
#14662=CARTESIAN_POINT('Ctrl Pts',(1.28758144276905,-1.07065491910773,9.79116853024056));
#14663=CARTESIAN_POINT('Ctrl Pts',(1.11666666666667,-0.338138082472195,
9.83333333333333));
#14664=CARTESIAN_POINT('Ctrl Pts',(1.11666666666667,-1.38777878078145E-16,
9.83333333333333));
#14665=CARTESIAN_POINT('Ctrl Pts',(1.28333333333333,8.55796914815225E-16,
9.66666666666667));
#14666=CARTESIAN_POINT('Ctrl Pts',(1.28333333333333,0.309230215187422,9.66666666666667));
#14667=CARTESIAN_POINT('Ctrl Pts',(1.38626480059327,0.808032798955786,9.64090067959512));
#14668=CARTESIAN_POINT('Ctrl Pts',(1.74096212275212,1.3726151324698,9.57118830316523));
#14669=CARTESIAN_POINT('Ctrl Pts',(2.17650323150611,1.83310440122169,9.49744847900364));
#14670=CARTESIAN_POINT('Ctrl Pts',(2.98881273415759,2.23510132776721,9.41140881531922));
#14671=CARTESIAN_POINT('Ctrl Pts',(4.01308321922153,2.23639823005159,9.41118892581281));
#14672=CARTESIAN_POINT('Ctrl Pts',(4.82214307889098,1.83015431700991,9.49763938587733));
#14673=CARTESIAN_POINT('Ctrl Pts',(5.25985229153288,1.37253372722753,9.57132841256933));
#14674=CARTESIAN_POINT('Ctrl Pts',(5.613684454071,0.799814157708089,9.64102974441768));
#14675=CARTESIAN_POINT('Ctrl Pts',(5.78520399585376,0.000200487986665598,
9.68389704026533));
#14676=CARTESIAN_POINT('Ctrl Pts',(5.61469740197354,-0.799079514653171,
9.6413036446087));
#14677=CARTESIAN_POINT('Ctrl Pts',(5.26030429887732,-1.37323364656096,9.57128832848508));
#14678=CARTESIAN_POINT('Ctrl Pts',(4.82148078742824,-1.82943889809227,9.49776749039775));
#14679=CARTESIAN_POINT('Ctrl Pts',(4.01531295778032,-2.23578316478115,9.41124961891846));
#14680=CARTESIAN_POINT('Ctrl Pts',(2.98388326589406,-2.23214984780108,9.41195776971814));
#14681=CARTESIAN_POINT('Ctrl Pts',(2.02366133578104,-1.75740995229055,9.5134504953496));
#14682=CARTESIAN_POINT('Ctrl Pts',(1.43656963770823,-0.979731881240677,
9.63085033926547));
#14683=CARTESIAN_POINT('Ctrl Pts',(1.28333333333333,-0.309230215187417,
9.66666666666667));
#14684=CARTESIAN_POINT('Ctrl Pts',(1.28333333333333,-1.38777878078145E-16,
9.66666666666667));
#14685=CARTESIAN_POINT('Ctrl Pts',(1.45,6.93889390390723E-16,9.5));
#14686=CARTESIAN_POINT('Ctrl Pts',(1.45,0.280322347902641,9.5));
#14687=CARTESIAN_POINT('Ctrl Pts',(1.54063609363717,0.732886734359709,9.47879413137563));
#14688=CARTESIAN_POINT('Ctrl Pts',(1.86134961790268,1.2550385025139,9.42030091871305));
#14689=CARTESIAN_POINT('Ctrl Pts',(2.25994381043875,1.68646294456639,9.35778808469502));
#14690=CARTESIAN_POINT('Ctrl Pts',(3.01739047190032,2.07176376570438,9.28365046104267));
#14691=CARTESIAN_POINT('Ctrl Pts',(3.98447117030109,2.07300467026798,9.28346232323077));
#14692=CARTESIAN_POINT('Ctrl Pts',(4.73876694008359,1.68376067730857,9.35793682465725));
#14693=CARTESIAN_POINT('Ctrl Pts',(5.13940112945,1.25495539919388,9.42041527554798));
#14694=CARTESIAN_POINT('Ctrl Pts',(5.45930066389954,0.725325638555357,9.47889707113072));
#14695=CARTESIAN_POINT('Ctrl Pts',(5.61031125091214,0.000164050414441131,
9.51417801609118));
#14696=CARTESIAN_POINT('Ctrl Pts',(5.46017502672277,-0.724598775406211,
9.47911924111307));
#14697=CARTESIAN_POINT('Ctrl Pts',(5.13981127341247,-1.2556046057082,9.42038049906894));
#14698=CARTESIAN_POINT('Ctrl Pts',(4.7381018704627,-1.68309041958779,9.35803831945692));
#14699=CARTESIAN_POINT('Ctrl Pts',(3.98639077283064,-2.07242961490702,9.28351496068093));
#14700=CARTESIAN_POINT('Ctrl Pts',(3.01292252447829,-2.06905273920491,9.28409180380522));
#14701=CARTESIAN_POINT('Ctrl Pts',(2.11712920026623,-1.61379783281266,9.37163046905901));
#14702=CARTESIAN_POINT('Ctrl Pts',(1.58555783264741,-0.888808843373621,
9.47053214829039));
#14703=CARTESIAN_POINT('Ctrl Pts',(1.45,-0.280322347902639,9.5));
#14704=CARTESIAN_POINT('Ctrl Pts',(1.45,-1.38777878078145E-16,9.5));
#14705=CARTESIAN_POINT('',(0.950000000000001,-1.38777878078145E-16,10.));
#14706=CARTESIAN_POINT('',(1.45,6.93889390390723E-16,9.5));
#14707=CARTESIAN_POINT('',(0.95,1.17961196366423E-15,10.));
#14708=CARTESIAN_POINT('Ctrl Pts',(1.45,6.93889390390723E-16,9.5));
#14709=CARTESIAN_POINT('Ctrl Pts',(1.45,0.280322347902641,9.5));
#14710=CARTESIAN_POINT('Ctrl Pts',(1.54063609363717,0.732886734359709,9.47879413137563));
#14711=CARTESIAN_POINT('Ctrl Pts',(1.86134961790268,1.2550385025139,9.42030091871305));
#14712=CARTESIAN_POINT('Ctrl Pts',(2.25994381043875,1.68646294456639,9.35778808469502));
#14713=CARTESIAN_POINT('Ctrl Pts',(3.01739047190032,2.07176376570438,9.28365046104267));
#14714=CARTESIAN_POINT('Ctrl Pts',(3.98447117030109,2.07300467026798,9.28346232323077));
#14715=CARTESIAN_POINT('Ctrl Pts',(4.73876694008359,1.68376067730857,9.35793682465725));
#14716=CARTESIAN_POINT('Ctrl Pts',(5.13940112945,1.25495539919388,9.42041527554798));
#14717=CARTESIAN_POINT('Ctrl Pts',(5.45930066389954,0.725325638555357,9.47889707113072));
#14718=CARTESIAN_POINT('Ctrl Pts',(5.61031125091214,0.000164050414441131,
9.51417801609118));
#14719=CARTESIAN_POINT('Ctrl Pts',(5.46017502672277,-0.724598775406211,
9.47911924111307));
#14720=CARTESIAN_POINT('Ctrl Pts',(5.13981127341247,-1.2556046057082,9.42038049906894));
#14721=CARTESIAN_POINT('Ctrl Pts',(4.7381018704627,-1.68309041958779,9.35803831945692));
#14722=CARTESIAN_POINT('Ctrl Pts',(3.98639077283064,-2.07242961490702,9.28351496068093));
#14723=CARTESIAN_POINT('Ctrl Pts',(3.01292252447829,-2.06905273920491,9.28409180380522));
#14724=CARTESIAN_POINT('Ctrl Pts',(2.11712920026623,-1.61379783281266,9.37163046905901));
#14725=CARTESIAN_POINT('Ctrl Pts',(1.58555783264741,-0.888808843373621,
9.47053214829039));
#14726=CARTESIAN_POINT('Ctrl Pts',(1.45,-0.280322347902639,9.5));
#14727=CARTESIAN_POINT('Ctrl Pts',(1.45,-1.38777878078145E-16,9.5));
#14728=CARTESIAN_POINT('Ctrl Pts',(0.950000000000001,-1.38777878078145E-16,
10.));
#14729=CARTESIAN_POINT('Ctrl Pts',(0.95,-0.367045949756973,10.));
#14730=CARTESIAN_POINT('Ctrl Pts',(1.13859324782988,-1.16157795697479,9.95148672121565));
#14731=CARTESIAN_POINT('Ctrl Pts',(1.83672560681065,-2.04463419124632,9.79709054793077));
#14732=CARTESIAN_POINT('Ctrl Pts',(2.9258047487256,-2.55834406499343,9.66768970154396));
#14733=CARTESIAN_POINT('Ctrl Pts',(4.07315732767968,-2.56249026452942,9.66671893539352));
#14734=CARTESIAN_POINT('Ctrl Pts',(4.98823862135932,-2.12213585510122,9.7772258322794));
#14735=CARTESIAN_POINT('Ctrl Pts',(5.50129034980703,-1.60849172826648,9.87310398731735));
#14736=CARTESIAN_POINT('Ctrl Pts',(5.92374215247507,-0.948040993147089,
9.96567245159996));
#14737=CARTESIAN_POINT('Ctrl Pts',(6.13498948573698,0.000273363131113907,
10.0233350886136));
#14738=CARTESIAN_POINT('Ctrl Pts',(5.92245203441391,0.948791196013554,9.9652950909916));
#14739=CARTESIAN_POINT('Ctrl Pts',(5.50075461569863,1.60769038329482,9.87315468661203));
#14740=CARTESIAN_POINT('Ctrl Pts',(4.98889535650575,2.12294159641258,9.77704450831748));
#14741=CARTESIAN_POINT('Ctrl Pts',(4.07030731706242,2.56318534961883,9.66664213097688));
#14742=CARTESIAN_POINT('Ctrl Pts',(2.93165725867213,2.56177645189286,9.6669255238723));
#14743=CARTESIAN_POINT('Ctrl Pts',(2.00962207364082,2.12638731453228,9.77676926762088));
#14744=CARTESIAN_POINT('Ctrl Pts',(1.50018713245098,1.6077683923816,9.87296307206958));
#14745=CARTESIAN_POINT('Ctrl Pts',(1.07752221450547,0.958324928147939,9.96511377603409));
#14746=CARTESIAN_POINT('Ctrl Pts',(0.95,0.367045949756984,10.));
#14747=CARTESIAN_POINT('Ctrl Pts',(0.95,1.17961196366423E-15,10.));
#14748=CARTESIAN_POINT('Origin',(3.5,0.,10.));
#14749=CARTESIAN_POINT('',(1.45,2.64304174990748E-16,5.025));
#14750=CARTESIAN_POINT('',(1.45,2.51052593825207E-16,10.));
#14751=CARTESIAN_POINT('',(3.5,2.05,4.58782355807195));
#14752=CARTESIAN_POINT('Ctrl Pts',(3.5,2.05,4.58782355807195));
#14753=CARTESIAN_POINT('Ctrl Pts',(3.23911658808884,2.05,4.58782355807195));
#14754=CARTESIAN_POINT('Ctrl Pts',(2.96327422636181,1.9972365364845,4.61243172108358));
#14755=CARTESIAN_POINT('Ctrl Pts',(2.4593022166293,1.78717027592319,4.6978188168031));
#14756=CARTESIAN_POINT('Ctrl Pts',(2.23085473008692,1.62999253295176,4.75702184253145));
#14757=CARTESIAN_POINT('Ctrl Pts',(1.87020630601552,1.26934410888037,4.86567773089675));
#14758=CARTESIAN_POINT('Ctrl Pts',(1.71287808635485,1.04082190467728,4.9226508378233));
#14759=CARTESIAN_POINT('Ctrl Pts',(1.50269621880289,0.536556350598789,5.00279010148928));
#14760=CARTESIAN_POINT('Ctrl Pts',(1.45,0.260595900858596,5.025));
#14761=CARTESIAN_POINT('Ctrl Pts',(1.45,4.16333634234434E-16,5.025));
#14762=CARTESIAN_POINT('Ctrl Pts',(1.45,2.77555756156289E-16,5.025));
#14763=CARTESIAN_POINT('Ctrl Pts',(1.45,-0.260595900858595,5.025));
#14764=CARTESIAN_POINT('Ctrl Pts',(1.50269621880289,-0.536556350598789,
5.00279010148928));
#14765=CARTESIAN_POINT('Ctrl Pts',(1.71287808635485,-1.04082190467728,4.9226508378233));
#14766=CARTESIAN_POINT('Ctrl Pts',(1.87020630601552,-1.26934410888037,4.86567773089675));
#14767=CARTESIAN_POINT('Ctrl Pts',(2.23085473008692,-1.62999253295176,4.75702184253145));
#14768=CARTESIAN_POINT('Ctrl Pts',(2.4593022166293,-1.78717027592319,4.6978188168031));
#14769=CARTESIAN_POINT('Ctrl Pts',(2.96327422636181,-1.9972365364845,4.61243172108358));
#14770=CARTESIAN_POINT('Ctrl Pts',(3.23911658808884,-2.05,4.58782355807195));
#14771=CARTESIAN_POINT('Ctrl Pts',(3.76088341191116,-2.05,4.58782355807195));
#14772=CARTESIAN_POINT('Ctrl Pts',(4.03672577363819,-1.9972365364845,4.61243172108358));
#14773=CARTESIAN_POINT('Ctrl Pts',(4.5406977833707,-1.78717027592319,4.6978188168031));
#14774=CARTESIAN_POINT('Ctrl Pts',(4.76914526991308,-1.62999253295176,4.75702184253145));
#14775=CARTESIAN_POINT('Ctrl Pts',(5.12979369398448,-1.26934410888037,4.86567773089675));
#14776=CARTESIAN_POINT('Ctrl Pts',(5.28712191364515,-1.04082190467728,4.9226508378233));
#14777=CARTESIAN_POINT('Ctrl Pts',(5.4973037811971,-0.53655635059879,5.00279010148928));
#14778=CARTESIAN_POINT('Ctrl Pts',(5.55,-0.260595900858596,5.025));
#14779=CARTESIAN_POINT('Ctrl Pts',(5.55,0.260595900858595,5.025));
#14780=CARTESIAN_POINT('Ctrl Pts',(5.4973037811971,0.53655635059879,5.00279010148928));
#14781=CARTESIAN_POINT('Ctrl Pts',(5.28712191364515,1.04082190467728,4.9226508378233));
#14782=CARTESIAN_POINT('Ctrl Pts',(5.12979369398448,1.26934410888037,4.86567773089675));
#14783=CARTESIAN_POINT('Ctrl Pts',(4.76914526991308,1.62999253295176,4.75702184253145));
#14784=CARTESIAN_POINT('Ctrl Pts',(4.5406977833707,1.78717027592319,4.6978188168031));
#14785=CARTESIAN_POINT('Ctrl Pts',(4.03672577363819,1.9972365364845,4.61243172108358));
#14786=CARTESIAN_POINT('Ctrl Pts',(3.76088341191116,2.05,4.58782355807195));
#14787=CARTESIAN_POINT('Ctrl Pts',(3.5,2.05,4.58782355807195));
#14788=CARTESIAN_POINT('Origin',(3.75,0.,0.));
#14789=CARTESIAN_POINT('',(7.,8.5,-5.26782687642637));
#14790=CARTESIAN_POINT('Origin',(15.5,0.,0.));
#14791=CARTESIAN_POINT('',(7.5,-8.,-6.));
#14792=CARTESIAN_POINT('Origin',(-0.5,0.,0.));
#14793=CARTESIAN_POINT('',(7.,-8.5,-5.26782687642637));
#14794=CARTESIAN_POINT('Origin',(15.5,0.,0.));
#14795=CARTESIAN_POINT('',(7.,-10.,-1.22464679914735E-15));
#14796=CARTESIAN_POINT('Origin',(7.,0.,0.));
#14797=CARTESIAN_POINT('',(0.5,-10.,-1.22464679914735E-15));
#14798=CARTESIAN_POINT('',(3.75,-10.,-1.22464679914735E-15));
#14799=CARTESIAN_POINT('Origin',(0.5,0.,0.));
#14800=CARTESIAN_POINT('',(7.,-8.5,5.26782687642637));
#14801=CARTESIAN_POINT('Origin',(7.,0.,0.));
#14802=CARTESIAN_POINT('Origin',(15.5,0.,0.));
#14803=CARTESIAN_POINT('',(7.5,8.,6.));
#14804=CARTESIAN_POINT('Origin',(-0.5,0.,0.));
#14805=CARTESIAN_POINT('',(7.,8.5,5.26782687642637));
#14806=CARTESIAN_POINT('Origin',(15.5,0.,0.));
#14807=CARTESIAN_POINT('Origin',(7.,0.,0.));
#14808=CARTESIAN_POINT('Origin',(12.,0.,0.));
#14809=CARTESIAN_POINT('',(12.,-5.025,-6.15385016571545E-16));
#14810=CARTESIAN_POINT('Origin',(12.,0.,0.));
#14811=CARTESIAN_POINT('Origin',(17.05,6.35,-18.));
#14812=CARTESIAN_POINT('',(16.7,6.,17.2310988842807));
#14813=CARTESIAN_POINT('',(17.,6.3,16.6381811916546));
#14814=CARTESIAN_POINT('Ctrl Pts',(16.7,6.,17.2310988842807));
#14815=CARTESIAN_POINT('Ctrl Pts',(16.865153077165,6.16515307716503,16.9346400379677));
#14816=CARTESIAN_POINT('Ctrl Pts',(17.,6.3,16.6381811916546));
#14817=CARTESIAN_POINT('',(16.7,6.,-17.2310988842807));
#14818=CARTESIAN_POINT('',(16.7,6.,-18.));
#14819=CARTESIAN_POINT('',(17.,6.3,-16.6381811916546));
#14820=CARTESIAN_POINT('Ctrl Pts',(17.,6.3,-16.6381811916546));
#14821=CARTESIAN_POINT('Ctrl Pts',(16.865153077165,6.16515307716504,-16.9346400379676));
#14822=CARTESIAN_POINT('Ctrl Pts',(16.7,6.,-17.2310988842807));
#14823=CARTESIAN_POINT('',(17.,6.3,-9.));
#14824=CARTESIAN_POINT('Origin',(16.7,6.,-18.));
#14825=CARTESIAN_POINT('',(17.,5.7,17.0594117081557));
#14826=CARTESIAN_POINT('Ctrl Pts',(17.,5.7,17.0594117081557));
#14827=CARTESIAN_POINT('Ctrl Pts',(16.8540939564508,5.84590604354921,17.1452552962182));
#14828=CARTESIAN_POINT('Ctrl Pts',(16.7,6.,17.2310988842807));
#14829=CARTESIAN_POINT('',(17.,5.7,-17.0594117081557));
#14830=CARTESIAN_POINT('',(17.,5.7,-9.));
#14831=CARTESIAN_POINT('Ctrl Pts',(16.7,6.,-17.2310988842807));
#14832=CARTESIAN_POINT('Ctrl Pts',(16.8540939564509,5.84590604354905,-17.1452552962181));
#14833=CARTESIAN_POINT('Ctrl Pts',(17.,5.7,-17.0594117081557));
#14834=CARTESIAN_POINT('Origin',(17.05,3.95,-18.));
#14835=CARTESIAN_POINT('',(16.7,3.6,17.8));
#14836=CARTESIAN_POINT('',(17.,3.9,17.5));
#14837=CARTESIAN_POINT('',(22.8666666666667,9.76666666666666,11.6333333333333));
#14838=CARTESIAN_POINT('',(16.7,3.6,-17.8));
#14839=CARTESIAN_POINT('',(16.7,3.6,-18.));
#14840=CARTESIAN_POINT('',(17.,3.9,-17.5));
#14841=CARTESIAN_POINT('',(15.5333333333333,2.43333333333334,-18.9666666666667));
#14842=CARTESIAN_POINT('',(17.,3.9,-9.));
#14843=CARTESIAN_POINT('Origin',(16.7,3.6,-18.));
#14844=CARTESIAN_POINT('',(17.,3.3,17.5));
#14845=CARTESIAN_POINT('',(22.6166666666667,-2.31666666666666,11.8833333333333));
#14846=CARTESIAN_POINT('',(17.,3.3,-17.5));
#14847=CARTESIAN_POINT('',(17.,3.3,-9.));
#14848=CARTESIAN_POINT('',(17.95,2.35000000000001,-16.55));
#14849=CARTESIAN_POINT('Origin',(17.05,1.55,-18.));
#14850=CARTESIAN_POINT('',(16.7,1.2,17.8));
#14851=CARTESIAN_POINT('',(17.,1.5,17.5));
#14852=CARTESIAN_POINT('',(23.2666666666667,7.76666666666666,11.2333333333333));
#14853=CARTESIAN_POINT('',(16.7,1.2,-17.8));
#14854=CARTESIAN_POINT('',(16.7,1.2,-18.));
#14855=CARTESIAN_POINT('',(17.,1.5,-17.5));
#14856=CARTESIAN_POINT('',(15.9333333333333,0.433333333333337,-18.5666666666667));
#14857=CARTESIAN_POINT('',(17.,1.5,-9.));
#14858=CARTESIAN_POINT('Origin',(16.7,1.2,-18.));
#14859=CARTESIAN_POINT('',(17.,0.900000000000001,17.5));
#14860=CARTESIAN_POINT('',(22.2166666666667,-4.31666666666666,12.2833333333333));
#14861=CARTESIAN_POINT('',(17.,0.900000000000001,-17.5));
#14862=CARTESIAN_POINT('',(17.,0.900000000000002,-9.));
#14863=CARTESIAN_POINT('',(17.55,0.350000000000006,-16.95));
#14864=CARTESIAN_POINT('Origin',(17.05,0.349999999999999,-18.));
#14865=CARTESIAN_POINT('',(16.7,-8.88178419700125E-16,17.8));
#14866=CARTESIAN_POINT('',(17.,0.299999999999999,17.5));
#14867=CARTESIAN_POINT('',(23.4666666666667,6.76666666666665,11.0333333333333));
#14868=CARTESIAN_POINT('',(16.7,-8.88178419700125E-16,-17.8));
#14869=CARTESIAN_POINT('',(16.7,-8.88178419700125E-16,-18.));
#14870=CARTESIAN_POINT('',(17.,0.299999999999998,-17.5));
#14871=CARTESIAN_POINT('',(16.1333333333333,-0.566666666666664,-18.3666666666667));
#14872=CARTESIAN_POINT('',(17.,0.299999999999998,-9.));
#14873=CARTESIAN_POINT('Origin',(16.7,-8.88178419700125E-16,-18.));
#14874=CARTESIAN_POINT('',(17.,-0.3,17.5));
#14875=CARTESIAN_POINT('',(22.0166666666667,-5.31666666666666,12.4833333333333));
#14876=CARTESIAN_POINT('',(17.,-0.3,-17.5));
#14877=CARTESIAN_POINT('',(17.,-0.299999999999999,-9.));
#14878=CARTESIAN_POINT('',(17.35,-0.649999999999996,-17.15));
#14879=CARTESIAN_POINT('Origin',(17.05,-2.05,-18.));
#14880=CARTESIAN_POINT('',(16.7,-2.4,17.8));
#14881=CARTESIAN_POINT('',(17.,-2.1,17.5));
#14882=CARTESIAN_POINT('',(23.8666666666667,4.76666666666666,10.6333333333333));
#14883=CARTESIAN_POINT('',(16.7,-2.4,-17.8));
#14884=CARTESIAN_POINT('',(16.7,-2.4,-18.));
#14885=CARTESIAN_POINT('',(17.,-2.1,-17.5));
#14886=CARTESIAN_POINT('',(16.5333333333333,-2.56666666666667,-17.9666666666667));
#14887=CARTESIAN_POINT('',(17.,-2.1,-9.));
#14888=CARTESIAN_POINT('Origin',(16.7,-2.4,-18.));
#14889=CARTESIAN_POINT('',(17.,-2.7,17.5));
#14890=CARTESIAN_POINT('',(21.6166666666667,-7.31666666666666,12.8833333333333));
#14891=CARTESIAN_POINT('',(17.,-2.7,-17.5));
#14892=CARTESIAN_POINT('',(17.,-2.7,-9.));
#14893=CARTESIAN_POINT('',(16.95,-2.65,-17.55));
#14894=CARTESIAN_POINT('Origin',(16.7,-4.8,-18.));
#14895=CARTESIAN_POINT('',(16.7,-4.8,-17.7148351242013));
#14896=CARTESIAN_POINT('',(17.,-5.1,-17.3226495451672));
#14897=CARTESIAN_POINT('Ctrl Pts',(16.7,-4.8,-17.7148351242013));
#14898=CARTESIAN_POINT('Ctrl Pts',(16.8583592135001,-4.95835921350012,-17.5187423346843));
#14899=CARTESIAN_POINT('Ctrl Pts',(17.,-5.1,-17.3226495451672));
#14900=CARTESIAN_POINT('',(16.7,-4.8,17.7148351242013));
#14901=CARTESIAN_POINT('',(16.7,-4.8,-18.));
#14902=CARTESIAN_POINT('',(17.,-5.1,17.3226495451672));
#14903=CARTESIAN_POINT('Ctrl Pts',(17.,-5.1,17.3226495451672));
#14904=CARTESIAN_POINT('Ctrl Pts',(16.8583592135001,-4.95835921350012,17.5187423346843));
#14905=CARTESIAN_POINT('Ctrl Pts',(16.7,-4.8,17.7148351242013));
#14906=CARTESIAN_POINT('',(17.,-5.1,-9.));
#14907=CARTESIAN_POINT('Origin',(17.05,-4.45,-18.));
#14908=CARTESIAN_POINT('',(17.,-4.5,-17.4641016151378));
#14909=CARTESIAN_POINT('Ctrl Pts',(17.,-4.5,-17.4641016151378));
#14910=CARTESIAN_POINT('Ctrl Pts',(16.8552389410473,-4.64476105895267,-17.5894683696695));
#14911=CARTESIAN_POINT('Ctrl Pts',(16.7,-4.8,-17.7148351242013));
#14912=CARTESIAN_POINT('',(17.,-4.5,17.4641016151378));
#14913=CARTESIAN_POINT('',(17.,-4.5,-9.));
#14914=CARTESIAN_POINT('Ctrl Pts',(16.7,-4.8,17.7148351242013));
#14915=CARTESIAN_POINT('Ctrl Pts',(16.8552389410473,-4.64476105895271,17.5894683696695));
#14916=CARTESIAN_POINT('Ctrl Pts',(17.,-4.5,17.4641016151378));
#14917=CARTESIAN_POINT('Origin',(16.7,-6.,-18.));
#14918=CARTESIAN_POINT('',(16.7,-6.,-17.2310988842807));
#14919=CARTESIAN_POINT('',(17.,-6.3,-16.6381811916546));
#14920=CARTESIAN_POINT('Ctrl Pts',(16.7,-6.,-17.2310988842807));
#14921=CARTESIAN_POINT('Ctrl Pts',(16.865153077165,-6.16515307716504,-16.9346400379676));
#14922=CARTESIAN_POINT('Ctrl Pts',(17.,-6.3,-16.6381811916546));
#14923=CARTESIAN_POINT('',(16.7,-6.,17.2310988842807));
#14924=CARTESIAN_POINT('',(16.7,-6.,-18.));
#14925=CARTESIAN_POINT('',(17.,-6.3,16.6381811916546));
#14926=CARTESIAN_POINT('Ctrl Pts',(17.,-6.3,16.6381811916546));
#14927=CARTESIAN_POINT('Ctrl Pts',(16.865153077165,-6.16515307716504,16.9346400379676));
#14928=CARTESIAN_POINT('Ctrl Pts',(16.7,-6.,17.2310988842807));
#14929=CARTESIAN_POINT('',(17.,-6.3,-9.));
#14930=CARTESIAN_POINT('Origin',(17.05,-5.65,-18.));
#14931=CARTESIAN_POINT('',(17.,-5.7,-17.0594117081557));
#14932=CARTESIAN_POINT('Ctrl Pts',(17.,-5.7,-17.0594117081557));
#14933=CARTESIAN_POINT('Ctrl Pts',(16.8540939564507,-5.84590604354931,-17.1452552962182));
#14934=CARTESIAN_POINT('Ctrl Pts',(16.7,-6.,-17.2310988842807));
#14935=CARTESIAN_POINT('',(17.,-5.7,17.0594117081557));
#14936=CARTESIAN_POINT('',(17.,-5.7,-9.));
#14937=CARTESIAN_POINT('Ctrl Pts',(16.7,-6.,17.2310988842807));
#14938=CARTESIAN_POINT('Ctrl Pts',(16.8540939564508,-5.84590604354915,17.1452552962182));
#14939=CARTESIAN_POINT('Ctrl Pts',(17.,-5.7,17.0594117081557));
#14940=CARTESIAN_POINT('Origin',(17.05,-3.25,-18.));
#14941=CARTESIAN_POINT('',(16.7,-3.6,17.8));
#14942=CARTESIAN_POINT('',(17.,-3.3,17.5));
#14943=CARTESIAN_POINT('',(24.0666666666667,3.76666666666665,10.4333333333333));
#14944=CARTESIAN_POINT('',(16.7,-3.6,-17.8));
#14945=CARTESIAN_POINT('',(16.7,-3.6,-18.));
#14946=CARTESIAN_POINT('',(17.,-3.3,-17.5));
#14947=CARTESIAN_POINT('',(16.7333333333333,-3.56666666666667,-17.7666666666667));
#14948=CARTESIAN_POINT('',(17.,-3.3,-9.));
#14949=CARTESIAN_POINT('Origin',(16.7,-3.6,-18.));
#14950=CARTESIAN_POINT('',(17.,-3.9,17.5));
#14951=CARTESIAN_POINT('',(21.4166666666667,-8.31666666666667,13.0833333333333));
#14952=CARTESIAN_POINT('',(17.,-3.9,-17.5));
#14953=CARTESIAN_POINT('',(17.,-3.9,-9.));
#14954=CARTESIAN_POINT('',(16.75,-3.65,-17.75));
#14955=CARTESIAN_POINT('Origin',(17.05,-0.85,-18.));
#14956=CARTESIAN_POINT('',(16.7,-1.2,17.8));
#14957=CARTESIAN_POINT('',(17.,-0.900000000000001,17.5));
#14958=CARTESIAN_POINT('',(23.6666666666667,5.76666666666665,10.8333333333333));
#14959=CARTESIAN_POINT('',(16.7,-1.2,-17.8));
#14960=CARTESIAN_POINT('',(16.7,-1.2,-18.));
#14961=CARTESIAN_POINT('',(17.,-0.900000000000001,-17.5));
#14962=CARTESIAN_POINT('',(16.3333333333333,-1.56666666666667,-18.1666666666667));
#14963=CARTESIAN_POINT('',(17.,-0.900000000000002,-9.));
#14964=CARTESIAN_POINT('Origin',(16.7,-1.2,-18.));
#14965=CARTESIAN_POINT('',(17.,-1.5,17.5));
#14966=CARTESIAN_POINT('',(21.8166666666667,-6.31666666666666,12.6833333333333));
#14967=CARTESIAN_POINT('',(17.,-1.5,-17.5));
#14968=CARTESIAN_POINT('',(17.,-1.5,-9.));
#14969=CARTESIAN_POINT('',(17.15,-1.65,-17.35));
#14970=CARTESIAN_POINT('Origin',(16.7,-7.2,-18.));
#14971=CARTESIAN_POINT('',(16.7,-7.2,-16.0493901531919));
#14972=CARTESIAN_POINT('',(17.,-7.5,-14.));
#14973=CARTESIAN_POINT('Ctrl Pts',(16.7,-7.2,-16.0493901531919));
#14974=CARTESIAN_POINT('Ctrl Pts',(17.,-7.5,-15.024695076596));
#14975=CARTESIAN_POINT('Ctrl Pts',(17.,-7.5,-14.));
#14976=CARTESIAN_POINT('',(16.7,-7.2,16.0493901531919));
#14977=CARTESIAN_POINT('',(16.7,-7.2,-18.));
#14978=CARTESIAN_POINT('',(17.,-7.5,14.));
#14979=CARTESIAN_POINT('Ctrl Pts',(17.,-7.5,14.));
#14980=CARTESIAN_POINT('Ctrl Pts',(17.,-7.5,15.024695076596));
#14981=CARTESIAN_POINT('Ctrl Pts',(16.7,-7.2,16.0493901531919));
#14982=CARTESIAN_POINT('',(17.,-7.5,9.));
#14983=CARTESIAN_POINT('Origin',(17.05,-6.85,-18.));
#14984=CARTESIAN_POINT('',(17.,-6.9,-15.9595917942265));
#14985=CARTESIAN_POINT('Ctrl Pts',(17.,-6.9,-15.9595917942265));
#14986=CARTESIAN_POINT('Ctrl Pts',(16.8533598938642,-7.04664010613577,-16.0044909737091));
#14987=CARTESIAN_POINT('Ctrl Pts',(16.7,-7.2,-16.0493901531919));
#14988=CARTESIAN_POINT('',(17.,-6.9,15.9595917942265));
#14989=CARTESIAN_POINT('',(17.,-6.9,-9.));
#14990=CARTESIAN_POINT('Ctrl Pts',(16.7,-7.2,16.0493901531919));
#14991=CARTESIAN_POINT('Ctrl Pts',(16.8533598938643,-7.04664010613571,16.004490973709));
#14992=CARTESIAN_POINT('Ctrl Pts',(17.,-6.9,15.9595917942265));
#14993=CARTESIAN_POINT('Origin',(17.05,2.75,-18.));
#14994=CARTESIAN_POINT('',(16.7,2.4,17.8));
#14995=CARTESIAN_POINT('',(17.,2.7,17.5));
#14996=CARTESIAN_POINT('',(23.0666666666667,8.76666666666666,11.4333333333333));
#14997=CARTESIAN_POINT('',(16.7,2.4,-17.8));
#14998=CARTESIAN_POINT('',(16.7,2.4,-18.));
#14999=CARTESIAN_POINT('',(17.,2.7,-17.5));
#15000=CARTESIAN_POINT('',(15.7333333333333,1.43333333333334,-18.7666666666667));
#15001=CARTESIAN_POINT('',(17.,2.7,-9.));
#15002=CARTESIAN_POINT('Origin',(16.7,2.4,-18.));
#15003=CARTESIAN_POINT('',(17.,2.1,17.5));
#15004=CARTESIAN_POINT('',(22.4166666666667,-3.31666666666666,12.0833333333333));
#15005=CARTESIAN_POINT('',(17.,2.1,-17.5));
#15006=CARTESIAN_POINT('',(17.,2.1,-9.));
#15007=CARTESIAN_POINT('',(17.75,1.35000000000001,-16.75));
#15008=CARTESIAN_POINT('Origin',(17.05,5.15,-18.));
#15009=CARTESIAN_POINT('',(16.7,4.8,17.7148351242013));
#15010=CARTESIAN_POINT('',(17.,5.1,17.3226495451672));
#15011=CARTESIAN_POINT('Ctrl Pts',(16.7,4.8,17.7148351242013));
#15012=CARTESIAN_POINT('Ctrl Pts',(16.8583592135001,4.95835921350012,17.5187423346843));
#15013=CARTESIAN_POINT('Ctrl Pts',(17.,5.1,17.3226495451672));
#15014=CARTESIAN_POINT('',(16.7,4.8,-17.7148351242013));
#15015=CARTESIAN_POINT('',(16.7,4.8,-18.));
#15016=CARTESIAN_POINT('',(17.,5.1,-17.3226495451672));
#15017=CARTESIAN_POINT('Ctrl Pts',(17.,5.1,-17.3226495451672));
#15018=CARTESIAN_POINT('Ctrl Pts',(16.8583592135001,4.95835921350012,-17.5187423346843));
#15019=CARTESIAN_POINT('Ctrl Pts',(16.7,4.8,-17.7148351242013));
#15020=CARTESIAN_POINT('',(17.,5.1,-9.));
#15021=CARTESIAN_POINT('Origin',(16.7,4.8,-18.));
#15022=CARTESIAN_POINT('',(17.,4.5,17.4641016151378));
#15023=CARTESIAN_POINT('Ctrl Pts',(17.,4.5,17.4641016151378));
#15024=CARTESIAN_POINT('Ctrl Pts',(16.8552389410473,4.64476105895274,17.5894683696696));
#15025=CARTESIAN_POINT('Ctrl Pts',(16.7,4.8,17.7148351242013));
#15026=CARTESIAN_POINT('',(17.,4.5,-17.4641016151378));
#15027=CARTESIAN_POINT('',(17.,4.5,-9.));
#15028=CARTESIAN_POINT('Ctrl Pts',(16.7,4.8,-17.7148351242013));
#15029=CARTESIAN_POINT('Ctrl Pts',(16.8552389410473,4.64476105895272,-17.5894683696695));
#15030=CARTESIAN_POINT('Ctrl Pts',(17.,4.5,-17.4641016151378));
#15031=CARTESIAN_POINT('Origin',(16.7,7.2,-18.));
#15032=CARTESIAN_POINT('',(16.7,7.2,-16.0493901531919));
#15033=CARTESIAN_POINT('',(17.,6.9,-15.9595917942265));
#15034=CARTESIAN_POINT('Ctrl Pts',(16.7,7.2,-16.0493901531919));
#15035=CARTESIAN_POINT('Ctrl Pts',(16.8533598938632,7.04664010613677,-16.0044909737094));
#15036=CARTESIAN_POINT('Ctrl Pts',(17.,6.9,-15.9595917942265));
#15037=CARTESIAN_POINT('',(16.7,7.2,16.0493901531919));
#15038=CARTESIAN_POINT('',(16.7,7.2,-18.));
#15039=CARTESIAN_POINT('',(17.,6.9,15.9595917942265));
#15040=CARTESIAN_POINT('Ctrl Pts',(17.,6.9,15.9595917942265));
#15041=CARTESIAN_POINT('Ctrl Pts',(16.8533598938628,7.04664010613721,16.0044909737095));
#15042=CARTESIAN_POINT('Ctrl Pts',(16.7,7.2,16.0493901531919));
#15043=CARTESIAN_POINT('',(17.,6.9,-9.));
#15044=CARTESIAN_POINT('Origin',(17.05,7.55,-18.));
#15045=CARTESIAN_POINT('',(17.,7.5,-14.));
#15046=CARTESIAN_POINT('Ctrl Pts',(17.,7.5,-14.));
#15047=CARTESIAN_POINT('Ctrl Pts',(17.,7.5,-15.024695076596));
#15048=CARTESIAN_POINT('Ctrl Pts',(16.7,7.2,-16.0493901531919));
#15049=CARTESIAN_POINT('',(17.,7.5,14.));
#15050=CARTESIAN_POINT('',(17.,7.5,-9.));
#15051=CARTESIAN_POINT('Ctrl Pts',(16.7,7.2,16.0493901531919));
#15052=CARTESIAN_POINT('Ctrl Pts',(17.,7.5,15.024695076596));
#15053=CARTESIAN_POINT('Ctrl Pts',(17.,7.5,14.));
#15054=CARTESIAN_POINT('Origin',(16.75,-4.,14.));
#15055=CARTESIAN_POINT('',(17.,-4.,17.5));
#15056=CARTESIAN_POINT('Origin',(17.,-4.,14.));
#15057=CARTESIAN_POINT('',(16.5,-4.,18.));
#15058=CARTESIAN_POINT('',(17.,-4.,17.5));
#15059=CARTESIAN_POINT('',(16.5,-8.,14.));
#15060=CARTESIAN_POINT('Origin',(16.5,-4.,14.));
#15061=CARTESIAN_POINT('',(17.,-7.5,14.));
#15062=CARTESIAN_POINT('Origin',(17.,-4.,14.));
#15063=CARTESIAN_POINT('Origin',(17.,-4.,14.));
#15064=CARTESIAN_POINT('Origin',(16.75,4.,17.75));
#15065=CARTESIAN_POINT('',(17.,4.,17.5));
#15066=CARTESIAN_POINT('',(17.,4.,17.5));
#15067=CARTESIAN_POINT('',(16.5,4.,18.));
#15068=CARTESIAN_POINT('',(17.,4.,17.5));
#15069=CARTESIAN_POINT('',(16.5,4.,18.));
#15070=CARTESIAN_POINT('',(17.,4.,17.5));
#15071=CARTESIAN_POINT('',(17.,4.,17.5));
#15072=CARTESIAN_POINT('',(17.,4.,17.5));
#15073=CARTESIAN_POINT('',(17.,4.,17.5));
#15074=CARTESIAN_POINT('',(17.,4.,17.5));
#15075=CARTESIAN_POINT('',(17.,4.,17.5));
#15076=CARTESIAN_POINT('',(17.,4.,17.5));
#15077=CARTESIAN_POINT('Origin',(17.,0.,0.));
#15078=CARTESIAN_POINT('Origin',(17.,4.,-14.));
#15079=CARTESIAN_POINT('Origin',(17.,4.,14.));
#15080=CARTESIAN_POINT('Origin',(17.,0.,0.));
#15081=CARTESIAN_POINT('',(17.,4.,-17.5));
#15082=CARTESIAN_POINT('',(17.,-4.,-17.5));
#15083=CARTESIAN_POINT('Origin',(17.,4.,-14.));
#15084=CARTESIAN_POINT('Origin',(17.,4.,14.));
#15085=CARTESIAN_POINT('Origin',(17.,0.,0.));
#15086=CARTESIAN_POINT('',(17.,-4.,-17.5));
#15087=CARTESIAN_POINT('Origin',(17.,0.,0.));
#15088=CARTESIAN_POINT('',(17.,-4.,-17.5));
#15089=CARTESIAN_POINT('Origin',(17.,0.,0.));
#15090=CARTESIAN_POINT('Origin',(17.,-4.,-14.));
#15091=CARTESIAN_POINT('Origin',(17.,0.,0.));
#15092=CARTESIAN_POINT('Origin',(17.,-4.,-14.));
#15093=CARTESIAN_POINT('Origin',(17.,0.,0.));
#15094=CARTESIAN_POINT('',(17.,-4.,-17.5));
#15095=CARTESIAN_POINT('Origin',(17.,-4.,-14.));
#15096=CARTESIAN_POINT('',(17.,-4.,-17.5));
#15097=CARTESIAN_POINT('Origin',(17.,0.,0.));
#15098=CARTESIAN_POINT('',(17.,-4.,-17.5));
#15099=CARTESIAN_POINT('Origin',(17.,0.,0.));
#15100=CARTESIAN_POINT('',(17.,-4.,-17.5));
#15101=CARTESIAN_POINT('Origin',(17.,0.,0.));
#15102=CARTESIAN_POINT('',(17.,-4.,-17.5));
#15103=CARTESIAN_POINT('Origin',(17.,0.,0.));
#15104=CARTESIAN_POINT('',(17.,-4.,-17.5));
#15105=CARTESIAN_POINT('Origin',(16.75,4.,14.));
#15106=CARTESIAN_POINT('',(16.5,8.,14.));
#15107=CARTESIAN_POINT('',(17.,7.5,14.));
#15108=CARTESIAN_POINT('Origin',(16.5,4.,14.));
#15109=CARTESIAN_POINT('Origin',(17.,4.,14.));
#15110=CARTESIAN_POINT('Origin',(7.25,-8.25,9.));
#15111=CARTESIAN_POINT('',(7.5,-8.,9.));
#15112=CARTESIAN_POINT('',(7.,-8.5,9.));
#15113=CARTESIAN_POINT('Origin',(7.,-8.,18.));
#15114=CARTESIAN_POINT('',(7.5,-8.,9.));
#15115=CARTESIAN_POINT('',(16.5,-8.,-14.));
#15116=CARTESIAN_POINT('',(7.,-8.,-14.));
#15117=CARTESIAN_POINT('',(16.5,-8.,9.));
#15118=CARTESIAN_POINT('',(7.,-8.,14.));
#15119=CARTESIAN_POINT('Origin',(7.25,8.25,-9.));
#15120=CARTESIAN_POINT('',(7.5,8.,-9.));
#15121=CARTESIAN_POINT('',(7.,8.5,-9.));
#15122=CARTESIAN_POINT('Origin',(7.,8.,-18.));
#15123=CARTESIAN_POINT('',(7.5,8.,-9.));
#15124=CARTESIAN_POINT('',(7.,8.,14.));
#15125=CARTESIAN_POINT('',(16.5,8.,-14.));
#15126=CARTESIAN_POINT('',(16.5,8.,-9.));
#15127=CARTESIAN_POINT('',(7.,8.,-14.));
#15128=CARTESIAN_POINT('Origin',(7.,-4.,14.));
#15129=CARTESIAN_POINT('',(7.,-4.,18.));
#15130=CARTESIAN_POINT('Origin',(7.25,-7.75,9.));
#15131=CARTESIAN_POINT('Origin',(7.,-4.,-14.));
#15132=CARTESIAN_POINT('',(16.5,-4.,-18.));
#15133=CARTESIAN_POINT('',(7.,-4.,-18.));
#15134=CARTESIAN_POINT('Origin',(16.5,-4.,-14.));
#15135=CARTESIAN_POINT('Origin',(7.25,7.75,-9.));
#15136=CARTESIAN_POINT('Origin',(7.,4.,-14.));
#15137=CARTESIAN_POINT('',(16.5,4.,-18.));
#15138=CARTESIAN_POINT('Origin',(16.5,4.,-14.));
#15139=CARTESIAN_POINT('',(7.,4.,-18.));
#15140=CARTESIAN_POINT('Origin',(7.,-8.,-18.));
#15141=CARTESIAN_POINT('',(16.5,-4.,-18.));
#15142=CARTESIAN_POINT('Origin',(16.75,-4.,-14.));
#15143=CARTESIAN_POINT('',(17.,-7.5,-14.));
#15144=CARTESIAN_POINT('',(16.5,-4.,-18.));
#15145=CARTESIAN_POINT('Origin',(16.75,-7.75,9.));
#15146=CARTESIAN_POINT('Origin',(16.75,7.75,-9.));
#15147=CARTESIAN_POINT('',(17.,7.5,-14.));
#15148=CARTESIAN_POINT('Origin',(16.75,4.,-14.));
#15149=CARTESIAN_POINT('Origin',(17.,4.,-14.));
#15150=CARTESIAN_POINT('',(17.,4.,-17.5));
#15151=CARTESIAN_POINT('Origin',(16.75,-4.,-17.75));
#15152=CARTESIAN_POINT('Origin',(17.,0.,0.));
#15153=CARTESIAN_POINT('Origin',(7.,4.,14.));
#15154=CARTESIAN_POINT('',(7.,4.,18.));
#15155=CARTESIAN_POINT('Origin',(7.,8.,18.));
#15156=CARTESIAN_POINT('Origin',(7.,5.025,0.));
#15157=CARTESIAN_POINT('Origin',(7.,5.025,0.));
#15158=CARTESIAN_POINT('Origin',(3.5,0.,0.));
#15159=CARTESIAN_POINT('',(0.,-5.025,-6.15385016571545E-16));
#15160=CARTESIAN_POINT('',(3.5,-5.025,-6.15385016571545E-16));
#15161=CARTESIAN_POINT('Origin',(0.,0.,0.));
#15162=CARTESIAN_POINT('Origin',(0.,9.5,0.));
#15163=CARTESIAN_POINT('',(-2.77555756156289E-16,-9.5,-1.16341445918999E-15));
#15164=CARTESIAN_POINT('Origin',(0.,0.,0.));
#15165=CARTESIAN_POINT('Origin',(0.25,0.,0.));
#15166=CARTESIAN_POINT('',(0.25,-9.75,-1.19403062916867E-15));
#15167=CARTESIAN_POINT('',(0.,0.,0.));
#15168=CARTESIAN_POINT('Origin',(2.1,0.,0.));
#15169=CARTESIAN_POINT('',(0.67986969212423,-1.9556340392028,0.00150612460811491));
#15170=CARTESIAN_POINT('',(0.57813030787577,-1.95561149193597,0.00205040622396644));
#15171=CARTESIAN_POINT('',(2.1,-1.954,-2.39295984553393E-16));
#15172=CARTESIAN_POINT('',(0.454,0.862538756400936,1.75492334225908));
#15173=CARTESIAN_POINT('Ctrl Pts',(0.67986969212423,-1.9556340392028,0.00150612460811491));
#15174=CARTESIAN_POINT('Ctrl Pts',(0.674641520753467,-1.95636945939027,
0.0929737669686619));
#15175=CARTESIAN_POINT('Ctrl Pts',(0.669413349382705,-1.95049672599127,
0.184341808759358));
#15176=CARTESIAN_POINT('Ctrl Pts',(0.664185178011942,-1.937688635782,0.274720676660528));
#15177=CARTESIAN_POINT('Ctrl Pts',(0.627496906321608,-1.84780889387837,
0.908947106032384));
#15178=CARTESIAN_POINT('Ctrl Pts',(0.590808634631275,-1.41640321821628,
1.49446248195575));
#15179=CARTESIAN_POINT('Ctrl Pts',(0.554120362940941,-0.837299495544021,
1.76873092177168));
#15180=CARTESIAN_POINT('Ctrl Pts',(0.520746908627294,-0.310518299782289,
2.01821896860936));
#15181=CARTESIAN_POINT('Ctrl Pts',(0.487373454313647,0.33847734856006,2.01016214817372));
#15182=CARTESIAN_POINT('Ctrl Pts',(0.454,0.863551653131349,1.75602537289061));
#15183=CARTESIAN_POINT('',(0.454,-0.861525859670523,1.75382131162755));
#15184=CARTESIAN_POINT('Origin',(0.454000000000001,0.,0.));
#15185=CARTESIAN_POINT('Ctrl Pts',(0.454,-0.861525859670525,1.75382131162755));
#15186=CARTESIAN_POINT('Ctrl Pts',(0.490688271690334,-1.4390822919413,1.47010951127397));
#15187=CARTESIAN_POINT('Ctrl Pts',(0.527376543380669,-1.86090523699116,
0.881484043774334));
#15188=CARTESIAN_POINT('Ctrl Pts',(0.564064815071003,-1.94128220444048,
0.246930232721736));
#15189=CARTESIAN_POINT('Ctrl Pts',(0.568753312672592,-1.95155380355776,
0.165838813471721));
#15190=CARTESIAN_POINT('Ctrl Pts',(0.573441810274181,-1.95624924699569,
0.0839973382522469));
#15191=CARTESIAN_POINT('Ctrl Pts',(0.57813030787577,-1.95561149193597,0.00205040622396644));
#15192=CARTESIAN_POINT('Origin',(2.1,0.,0.));
#15193=CARTESIAN_POINT('',(1.37986969212423,-1.95093233439697,-2.27181786092989E-5));
#15194=CARTESIAN_POINT('',(1.27813030787577,-1.95093620579234,0.000136491009683568));
#15195=CARTESIAN_POINT('',(2.1,-1.954,-2.39295984553393E-16));
#15196=CARTESIAN_POINT('Ctrl Pts',(1.37986969212423,-1.95093233439697,-2.27181786092989E-5));
#15197=CARTESIAN_POINT('Ctrl Pts',(1.36143781756214,-1.95089544086302,0.324452095312547));
#15198=CARTESIAN_POINT('Ctrl Pts',(1.34300594300005,-1.8741920465679,0.648942870541793));
#15199=CARTESIAN_POINT('Ctrl Pts',(1.32457406843796,-1.72092037455472,0.931966401256464));
#15200=CARTESIAN_POINT('Ctrl Pts',(1.28788579674762,-1.41583622663974,1.49531898672669));
#15201=CARTESIAN_POINT('Ctrl Pts',(1.25119752505729,-0.807387847480595,
1.89437796224664));
#15202=CARTESIAN_POINT('Ctrl Pts',(1.21450925336695,-0.169124111500478,
1.94974527786031));
#15203=CARTESIAN_POINT('Ctrl Pts',(1.17782098167662,0.469139624479642,2.00511259347399));
#15204=CARTESIAN_POINT('Ctrl Pts',(1.14113270998628,1.13721871728073,1.71678824918138));
#15205=CARTESIAN_POINT('Ctrl Pts',(1.10444443829595,1.53474739736028,1.21437219896546));
#15206=CARTESIAN_POINT('Ctrl Pts',(1.06775616660562,1.93227607743982,0.711956148749533));
#15207=CARTESIAN_POINT('Ctrl Pts',(1.03106789491528,2.05925434479783,-0.00455160738971262));
#15208=CARTESIAN_POINT('Ctrl Pts',(0.994379623224949,1.85860375663964,-0.612964951193619));
#15209=CARTESIAN_POINT('Ctrl Pts',(0.957691351534615,1.65795316848146,-1.22137829499753));
#15210=CARTESIAN_POINT('Ctrl Pts',(0.92100307984428,1.12967372480708,-1.72169722646609));
#15211=CARTESIAN_POINT('Ctrl Pts',(0.884314808153946,0.51125562378511,-1.8890841189366));
#15212=CARTESIAN_POINT('Ctrl Pts',(0.847626536463612,-0.107162477236863,
-2.05647101140711));
#15213=CARTESIAN_POINT('Ctrl Pts',(0.810938264773279,-0.815719235606428,
-1.89092586487956));
#15214=CARTESIAN_POINT('Ctrl Pts',(0.774249993082945,-1.29582071071862,
-1.46668455020561));
#15215=CARTESIAN_POINT('Ctrl Pts',(0.742789892763374,-1.70750651314859,
-1.10289869427864));
#15216=CARTESIAN_POINT('Ctrl Pts',(0.711329792443802,-1.95120870743107,
-0.548893049517983));
#15217=CARTESIAN_POINT('Ctrl Pts',(0.67986969212423,-1.9556340392028,0.00150612460811491));
#15218=CARTESIAN_POINT('Ctrl Pts',(0.57813030787577,-1.95561149193597,0.00205040622396644));
#15219=CARTESIAN_POINT('Ctrl Pts',(0.610130081964515,-1.95125870783131,
-0.557251002244683));
#15220=CARTESIAN_POINT('Ctrl Pts',(0.642129856053259,-1.69847012498212,
-1.1214648936334));
#15221=CARTESIAN_POINT('Ctrl Pts',(0.674129630142004,-1.27449056660128,
-1.48565001922452));
#15222=CARTESIAN_POINT('Ctrl Pts',(0.710817901832338,-0.788390971463978,
-1.90319430551263));
#15223=CARTESIAN_POINT('Ctrl Pts',(0.747506173522672,-0.0772607913405855,
-2.05780072348329));
#15224=CARTESIAN_POINT('Ctrl Pts',(0.784194445213007,0.538717801437386,
-1.88129345403462));
#15225=CARTESIAN_POINT('Ctrl Pts',(0.820882716903341,1.15469639421536,-1.70478618458595));
#15226=CARTESIAN_POINT('Ctrl Pts',(0.857570988593675,1.67552339964791,-1.19716522771797));
#15227=CARTESIAN_POINT('Ctrl Pts',(0.894259260284009,1.86728135704296,-0.585977319686521));
#15228=CARTESIAN_POINT('Ctrl Pts',(0.930947531974343,2.05903931443802,0.0252105883449238));
#15229=CARTESIAN_POINT('Ctrl Pts',(0.967635803664677,1.92172822379558,0.739965447539829));
#15230=CARTESIAN_POINT('Ctrl Pts',(1.00432407535501,1.51695619911708,1.23659176882114));
#15231=CARTESIAN_POINT('Ctrl Pts',(1.04101234704534,1.11218417443858,1.73321809010245));
#15232=CARTESIAN_POINT('Ctrl Pts',(1.07770061873568,0.439951215724031,2.01171587347017));
#15233=CARTESIAN_POINT('Ctrl Pts',(1.11438889042601,-0.197448824726387,
1.94705834975702));
#15234=CARTESIAN_POINT('Ctrl Pts',(1.15107716211635,-0.834848865176806,
1.88240082604387));
#15235=CARTESIAN_POINT('Ctrl Pts',(1.18776543380668,-1.43741598736309,1.47458799524984));
#15236=CARTESIAN_POINT('Ctrl Pts',(1.22445370549701,-1.73427713098456,0.90687236394884));
#15237=CARTESIAN_POINT('Ctrl Pts',(1.24234590628993,-1.87905089503979,0.630007807497356));
#15238=CARTESIAN_POINT('Ctrl Pts',(1.26023810708285,-1.95111753748238,0.315113008990274));
#15239=CARTESIAN_POINT('Ctrl Pts',(1.27813030787577,-1.95093620579234,0.000136491009683568));
#15240=CARTESIAN_POINT('Origin',(2.1,0.,0.));
#15241=CARTESIAN_POINT('',(2.07986969212423,-1.95573740044118,-0.00134534213615312));
#15242=CARTESIAN_POINT('',(1.97813030787577,-1.95548811205351,-0.0014374884722698));
#15243=CARTESIAN_POINT('',(2.1,-1.954,-2.39295984553393E-16));
#15244=CARTESIAN_POINT('Ctrl Pts',(2.07986969212423,-1.95573740044118,-0.00134534213615312));
#15245=CARTESIAN_POINT('Ctrl Pts',(2.04823411437081,-1.9513617754685,0.552080435026859));
#15246=CARTESIAN_POINT('Ctrl Pts',(2.01659853661739,-1.70457952528747,1.10892355752443));
#15247=CARTESIAN_POINT('Ctrl Pts',(1.98496295886397,-1.28886598803054,1.47273565024201));
#15248=CARTESIAN_POINT('Ctrl Pts',(1.94827468717363,-0.806756531420955,
1.89465419416391));
#15249=CARTESIAN_POINT('Ctrl Pts',(1.9115864154833,-0.0974446001355302,
2.05695755125819));
#15250=CARTESIAN_POINT('Ctrl Pts',(1.87489814379296,0.520171110472839,1.88667626129182));
#15251=CARTESIAN_POINT('Ctrl Pts',(1.83820987210263,1.13778682108121,1.71639497132545));
#15252=CARTESIAN_POINT('Ctrl Pts',(1.8015216004123,1.66370631101252,1.21352903429844));
#15253=CARTESIAN_POINT('Ctrl Pts',(1.76483332872196,1.8614821267408,0.60416070898101));
#15254=CARTESIAN_POINT('Ctrl Pts',(1.72814505703163,2.05925794246908,-0.00520761633642043));
#15255=CARTESIAN_POINT('Ctrl Pts',(1.69145678534129,1.92889008399431,-0.721078329944262));
#15256=CARTESIAN_POINT('Ctrl Pts',(1.65476851365096,1.52899061373608,-1.22160301259317));
#15257=CARTESIAN_POINT('Ctrl Pts',(1.61808024196063,1.12909114347786,-1.72212769524207));
#15258=CARTESIAN_POINT('Ctrl Pts',(1.58139197027029,0.459660061436177,-2.00730634693204));
#15259=CARTESIAN_POINT('Ctrl Pts',(1.54470369857996,-0.178334368785628,
-1.94892793551582));
#15260=CARTESIAN_POINT('Ctrl Pts',(1.50801542688963,-0.816328799007432,
-1.89054952409961));
#15261=CARTESIAN_POINT('Ctrl Pts',(1.47132715519929,-1.42288657740936,-1.48861404957721));
#15262=CARTESIAN_POINT('Ctrl Pts',(1.43463888350896,-1.72530550827492,-0.923823214605753));
#15263=CARTESIAN_POINT('Ctrl Pts',(1.41638248638071,-1.87579174942525,-0.642778474622892));
#15264=CARTESIAN_POINT('Ctrl Pts',(1.39812608925247,-1.9509688766925,-0.321408426032222));
#15265=CARTESIAN_POINT('Ctrl Pts',(1.37986969212423,-1.95093233439697,-2.27181786092989E-5));
#15266=CARTESIAN_POINT('Ctrl Pts',(1.27813030787577,-1.95093620579234,0.000136491009683568));
#15267=CARTESIAN_POINT('Ctrl Pts',(1.29692637877319,-1.95074571367002,-0.330751868198069));
#15268=CARTESIAN_POINT('Ctrl Pts',(1.3157224496706,-1.87082328801285,-0.661730411964054));
#15269=CARTESIAN_POINT('Ctrl Pts',(1.33451852056802,-1.71170123577323,-0.948803989963511));
#15270=CARTESIAN_POINT('Ctrl Pts',(1.37120679225835,-1.40110903188379,-1.50914628076687));
#15271=CARTESIAN_POINT('Ctrl Pts',(1.40789506394869,-0.788769459048261,
-1.9022124305656));
#15272=CARTESIAN_POINT('Ctrl Pts',(1.44458333563902,-0.149992814154617,
-1.9513104881624));
#15273=CARTESIAN_POINT('Ctrl Pts',(1.48127160732935,0.488783830739032,-2.00040854575921));
#15274=CARTESIAN_POINT('Ctrl Pts',(1.51795987901969,1.15399754769079,-1.70553851115407));
#15275=CARTESIAN_POINT('Ctrl Pts',(1.55464815071002,1.54658070225749,-1.19925693841763));
#15276=CARTESIAN_POINT('Ctrl Pts',(1.59133642240036,1.93916385682417,-0.692975365681195));
#15277=CARTESIAN_POINT('Ctrl Pts',(1.62802469409069,2.0591164490058,0.0247177451865357));
#15278=CARTESIAN_POINT('Ctrl Pts',(1.66471296578102,1.85250659557346,0.631148569663603));
#15279=CARTESIAN_POINT('Ctrl Pts',(1.70140123747136,1.64589674214113,1.23757939414067));
#15280=CARTESIAN_POINT('Ctrl Pts',(1.73808950916169,1.11272444309483,1.73274793222708));
#15281=CARTESIAN_POINT('Ctrl Pts',(1.77477778085203,0.492699242176483,1.89403577002722));
#15282=CARTESIAN_POINT('Ctrl Pts',(1.81146605254236,-0.127325958741865,
2.05532360782735));
#15283=CARTESIAN_POINT('Ctrl Pts',(1.84815432423269,-0.834204061532267,
1.88273074534122));
#15284=CARTESIAN_POINT('Ctrl Pts',(1.88484259592303,-1.3101313749037,1.45385101633328));
#15285=CARTESIAN_POINT('Ctrl Pts',(1.91593849990727,-1.71351341930723,1.09034512577004));
#15286=CARTESIAN_POINT('Ctrl Pts',(1.94703440389152,-1.95098593971063,0.542728879320629));
#15287=CARTESIAN_POINT('Ctrl Pts',(1.97813030787577,-1.95548811205351,-0.0014374884722698));
#15288=CARTESIAN_POINT('Origin',(2.1,0.,0.));
#15289=CARTESIAN_POINT('',(2.77986969212423,-1.95420215314675,0.00168616502236846));
#15290=CARTESIAN_POINT('',(2.67813030787577,-1.95448068520311,0.00166033696128984));
#15291=CARTESIAN_POINT('',(2.1,-1.954,-2.39295984553393E-16));
#15292=CARTESIAN_POINT('Ctrl Pts',(2.77986969212423,-1.95420215314675,0.00168616502236846));
#15293=CARTESIAN_POINT('Ctrl Pts',(2.77171868286981,-1.95547750749154,0.144568567579198));
#15294=CARTESIAN_POINT('Ctrl Pts',(2.7635676736154,-1.94110534109393,0.287196450375289));
#15295=CARTESIAN_POINT('Ctrl Pts',(2.75541666436098,-1.91011366966327,0.426116630272658));
#15296=CARTESIAN_POINT('Ctrl Pts',(2.71872839267065,-1.77061795494924,1.05140622868445));
#15297=CARTESIAN_POINT('Ctrl Pts',(2.68204012098031,-1.29441704307028,1.60157909930793));
#15298=CARTESIAN_POINT('Ctrl Pts',(2.64535184928998,-0.695590903406722,
1.82928445128862));
#15299=CARTESIAN_POINT('Ctrl Pts',(2.60866357759965,-0.0967647637431678,
2.0569898032693));
#15300=CARTESIAN_POINT('Ctrl Pts',(2.57197530590931,0.624686603704984,1.96222763660718));
#15301=CARTESIAN_POINT('Ctrl Pts',(2.53528703421898,1.14439923861265,1.58760159088831));
#15302=CARTESIAN_POINT('Ctrl Pts',(2.49859876252864,1.66411187352032,1.21297554516944));
#15303=CARTESIAN_POINT('Ctrl Pts',(2.46191049083831,1.98208577588749,0.558485620393793));
#15304=CARTESIAN_POINT('Ctrl Pts',(2.42522221914798,1.95536747148768,-0.0816167652630086));
#15305=CARTESIAN_POINT('Ctrl Pts',(2.38853394745764,1.92864916708787,-0.721719150919808));
#15306=CARTESIAN_POINT('Ctrl Pts',(2.35184567576731,1.55723865592108,-1.34743399745777));
#15307=CARTESIAN_POINT('Ctrl Pts',(2.31515740407697,1.00811580676684,-1.67744708930463));
#15308=CARTESIAN_POINT('Ctrl Pts',(2.27846913238664,0.458992957612606,-2.0074601811515));
#15309=CARTESIAN_POINT('Ctrl Pts',(2.24178086069631,-0.267842229529066,
-2.04177151830727));
#15310=CARTESIAN_POINT('Ctrl Pts',(2.20509258900597,-0.845611821739383,
-1.76495510350447));
#15311=CARTESIAN_POINT('Ctrl Pts',(2.16840431731564,-1.4233814139497,-1.48813868870167));
#15312=CARTESIAN_POINT('Ctrl Pts',(2.1317160456253,-1.85208541122867,-0.900194521940303));
#15313=CARTESIAN_POINT('Ctrl Pts',(2.09502777393497,-1.93898391890127,-0.265455573184856));
#15314=CARTESIAN_POINT('Ctrl Pts',(2.08997507999806,-1.9509515462278,-0.178039581911978));
#15315=CARTESIAN_POINT('Ctrl Pts',(2.08492238606114,-1.95643625582299,-0.0897360486564587));
#15316=CARTESIAN_POINT('Ctrl Pts',(2.07986969212423,-1.95573740044118,-0.00134534213615312));
#15317=CARTESIAN_POINT('Ctrl Pts',(1.97813030787577,-1.95548811205351,-0.0014374884722698));
#15318=CARTESIAN_POINT('Ctrl Pts',(1.98372267558186,-1.95629779435862,-0.0993017738625638));
#15319=CARTESIAN_POINT('Ctrl Pts',(1.98931504328794,-1.94957243403652,-0.197054478603423));
#15320=CARTESIAN_POINT('Ctrl Pts',(1.99490741099403,-1.93492195755465,-0.29360461873689));
#15321=CARTESIAN_POINT('Ctrl Pts',(2.03159568268436,-1.83880870288169,-0.927013929269352));
#15322=CARTESIAN_POINT('Ctrl Pts',(2.0682839543747,-1.40160566958331,-1.50866595480452));
#15323=CARTESIAN_POINT('Ctrl Pts',(2.10497222606503,-0.819874489822593,
-1.77705709146748));
#15324=CARTESIAN_POINT('Ctrl Pts',(2.14166049775537,-0.238143310061873,
-2.04544822813044));
#15325=CARTESIAN_POINT('Ctrl Pts',(2.1783487694457,0.488116016161189,-2.00057847592119));
#15326=CARTESIAN_POINT('Ctrl Pts',(2.21503704113603,1.0323854857134,-1.66262046846173));
#15327=CARTESIAN_POINT('Ctrl Pts',(2.25172531282637,1.57665495526561,-1.32466246100228));
#15328=CARTESIAN_POINT('Ctrl Pts',(2.2884135845167,1.93893456814697,-0.693616198292611));
#15329=CARTESIAN_POINT('Ctrl Pts',(2.32510185620704,1.95634776555644,-0.0531930972874931));
#15330=CARTESIAN_POINT('Ctrl Pts',(2.36179012789737,1.97376096296591,0.587230003717631));
#15331=CARTESIAN_POINT('Ctrl Pts',(2.39847839958771,1.64630774490349,1.23702994301821));
#15332=CARTESIAN_POINT('Ctrl Pts',(2.43516667127804,1.12120682401803,1.60406418566906));
#15333=CARTESIAN_POINT('Ctrl Pts',(2.47185494296837,0.596105903132565,1.97109842831991));
#15334=CARTESIAN_POINT('Ctrl Pts',(2.50854321465871,-0.126642720575935,
2.05536697432103));
#15335=CARTESIAN_POINT('Ctrl Pts',(2.54523148634904,-0.722098404848319,
1.81898347736198));
#15336=CARTESIAN_POINT('Ctrl Pts',(2.58191975803937,-1.3175540891207,1.58259998040294));
#15337=CARTESIAN_POINT('Ctrl Pts',(2.61860802972971,-1.78571683395696,1.02556444048373));
#15338=CARTESIAN_POINT('Ctrl Pts',(2.65529630142004,-1.91610803996687,0.398313972336145));
#15339=CARTESIAN_POINT('Ctrl Pts',(2.66290763690529,-1.94315895208515,0.268184818620666));
#15340=CARTESIAN_POINT('Ctrl Pts',(2.67051897239053,-1.95567234588532,0.135033649465785));
#15341=CARTESIAN_POINT('Ctrl Pts',(2.67813030787577,-1.95448068520311,0.00166033696128984));
#15342=CARTESIAN_POINT('Origin',(2.1,0.,0.));
#15343=CARTESIAN_POINT('',(3.47986969212423,-1.95164700307266,-0.000819222043828699));
#15344=CARTESIAN_POINT('',(3.37813030787577,-1.95121195149822,-0.0006614001062776));
#15345=CARTESIAN_POINT('',(2.1,-1.954,-2.39295984553393E-16));
#15346=CARTESIAN_POINT('Ctrl Pts',(3.47986969212423,-1.95164700307266,-0.000819222043828699));
#15347=CARTESIAN_POINT('Ctrl Pts',(3.45851497967848,-1.95006730859878,0.374954087447911));
#15348=CARTESIAN_POINT('Ctrl Pts',(3.43716026723274,-1.84503254302502,0.751463634279672));
#15349=CARTESIAN_POINT('Ctrl Pts',(3.41580555478699,-1.64211448138342,1.06439633074359));
#15350=CARTESIAN_POINT('Ctrl Pts',(3.37911728309666,-1.29349293027158,1.60202753593197));
#15351=CARTESIAN_POINT('Ctrl Pts',(3.34242901140633,-0.655952689440626,
1.95200118316467));
#15352=CARTESIAN_POINT('Ctrl Pts',(3.30574073971599,-0.0154087903711613,
1.95700568946614));
#15353=CARTESIAN_POINT('Ctrl Pts',(3.26905246802566,0.625135108698308,1.96201019576761));
#15354=CARTESIAN_POINT('Ctrl Pts',(3.23236419633532,1.26868266600629,1.62204556113784));
#15355=CARTESIAN_POINT('Ctrl Pts',(3.19567592464499,1.62553032427784,1.08993855285164));
#15356=CARTESIAN_POINT('Ctrl Pts',(3.15898765295466,1.98237798254938,0.557831544565436));
#15357=CARTESIAN_POINT('Ctrl Pts',(3.12229938126432,2.0525257417845,-0.166417837377206));
#15358=CARTESIAN_POINT('Ctrl Pts',(3.08561110957399,1.80463024676985,-0.757186102430425));
#15359=CARTESIAN_POINT('Ctrl Pts',(3.04892283788365,1.55673475175519,-1.34795436748365));
#15360=CARTESIAN_POINT('Ctrl Pts',(3.01223456619332,0.99079600249076,-1.80524151564745));
#15361=CARTESIAN_POINT('Ctrl Pts',(2.97554629450299,0.361152015741564,-1.92346124918403));
#15362=CARTESIAN_POINT('Ctrl Pts',(2.93885802281265,-0.268491971007628,
-2.04168098272061));
#15363=CARTESIAN_POINT('Ctrl Pts',(2.90216975112232,-0.961841195241583,
-1.82083330162998));
#15364=CARTESIAN_POINT('Ctrl Pts',(2.86548147943198,-1.407120548584,-1.36020629798461));
#15365=CARTESIAN_POINT('Ctrl Pts',(2.83694421699607,-1.75347248009176,-1.00191649357386));
#15366=CARTESIAN_POINT('Ctrl Pts',(2.80840695456015,-1.94973704698626,-0.498555276493542));
#15367=CARTESIAN_POINT('Ctrl Pts',(2.77986969212423,-1.95420215314675,0.00168616502236846));
#15368=CARTESIAN_POINT('Ctrl Pts',(2.67813030787577,-1.95448068520311,0.00166033696128984));
#15369=CARTESIAN_POINT('Ctrl Pts',(2.70720724408086,-1.94992828546958,-0.507854360777897));
#15370=CARTESIAN_POINT('Ctrl Pts',(2.73628418028595,-1.74536376071737,-1.02061102763673));
#15371=CARTESIAN_POINT('Ctrl Pts',(2.76536111649104,-1.38719894302305,-1.38051015791529));
#15372=CARTESIAN_POINT('Ctrl Pts',(2.80204938818138,-0.935278972885786,
-1.8346184236432));
#15373=CARTESIAN_POINT('Ctrl Pts',(2.83873765987171,-0.23881936542771,-2.04536955872304));
#15374=CARTESIAN_POINT('Ctrl Pts',(2.87542593156205,0.389052003290823,-1.9180113690157));
#15375=CARTESIAN_POINT('Ctrl Pts',(2.91211420325238,1.01692337200935,-1.79065317930836));
#15376=CARTESIAN_POINT('Ctrl Pts',(2.94880247494271,1.57620650198834,-1.32518566481383));
#15377=CARTESIAN_POINT('Ctrl Pts',(2.98549074663305,1.81546846933065,-0.730879403442768));
#15378=CARTESIAN_POINT('Ctrl Pts',(3.02217901832338,2.05473043667296,-0.136573142071704));
#15379=CARTESIAN_POINT('Ctrl Pts',(3.05886729001372,1.97397124137859,0.586571866175893));
#15380=CARTESIAN_POINT('Ctrl Pts',(3.09555556170405,1.60947172480172,1.11344101728923));
#15381=CARTESIAN_POINT('Ctrl Pts',(3.13224383339438,1.24497220822485,1.64031016840256));
#15382=CARTESIAN_POINT('Ctrl Pts',(3.16893210508472,0.596732370365471,1.97090346238163));
#15383=CARTESIAN_POINT('Ctrl Pts',(3.20562037677505,-0.0437537922871413,
1.9565838232007));
#15384=CARTESIAN_POINT('Ctrl Pts',(3.24230864846539,-0.684239954939754,
1.94226418401977));
#15385=CARTESIAN_POINT('Ctrl Pts',(3.27899692015572,-1.3169724423856,1.58303161167885));
#15386=CARTESIAN_POINT('Ctrl Pts',(3.31568519184605,-1.65758271925546,1.04040462540785));
#15387=CARTESIAN_POINT('Ctrl Pts',(3.33650023052263,-1.85082747459649,0.732545977785637));
#15388=CARTESIAN_POINT('Ctrl Pts',(3.3573152691992,-1.95004264571188,0.365655528174976));
#15389=CARTESIAN_POINT('Ctrl Pts',(3.37813030787577,-1.95121195149822,-0.0006614001062776));
#15390=CARTESIAN_POINT('Origin',(-0.840056225603703,0.,0.));
#15391=CARTESIAN_POINT('',(3.7099437743963,-1.55362687475922,-0.0006521493803482));
#15392=CARTESIAN_POINT('',(3.746,-1.5555,-7.61108830709034E-15));
#15393=CARTESIAN_POINT('',(-0.840056225603703,-1.5555,-7.61108830709034E-15));
#15394=CARTESIAN_POINT('',(3.746,-1.47474487035273,-0.49467950975182));
#15395=CARTESIAN_POINT('Ctrl Pts',(3.7099437743963,-1.55362687475922,-0.000652149380348192));
#15396=CARTESIAN_POINT('Ctrl Pts',(3.7219625162642,-1.55433463120761,-0.169011276618047));
#15397=CARTESIAN_POINT('Ctrl Pts',(3.7339812581321,-1.52895516772819,-0.337184754324949));
#15398=CARTESIAN_POINT('Ctrl Pts',(3.746,-1.47669774220803,-0.496045317568146));
#15399=CARTESIAN_POINT('Origin',(3.746,0.,0.));
#15400=CARTESIAN_POINT('Origin',(-0.840056225603703,0.,0.));
#15401=CARTESIAN_POINT('',(3.0099437743963,-1.55566092590572,0.00134228745768336));
#15402=CARTESIAN_POINT('',(3.1480562256037,-1.55328054787896,-0.000526513748883434));
#15403=CARTESIAN_POINT('',(-0.840056225603703,-1.5555,-7.61108830709034E-15));
#15404=CARTESIAN_POINT('Ctrl Pts',(3.0099437743963,-1.55566092590572,0.00134228745768327));
#15405=CARTESIAN_POINT('Ctrl Pts',(3.03848103683221,-1.55210643632913,-0.396879597024407));
#15406=CARTESIAN_POINT('Ctrl Pts',(3.10370657095846,-1.19500410016139,-1.31274265575085));
#15407=CARTESIAN_POINT('Ctrl Pts',(3.20562037677505,0.33821159539077,-1.80110713232262));
#15408=CARTESIAN_POINT('Ctrl Pts',(3.31568519184605,1.6897741201822,-0.709023981398171));
#15409=CARTESIAN_POINT('Ctrl Pts',(3.42575000691706,1.52224877807848,1.02061252875298));
#15410=CARTESIAN_POINT('Ctrl Pts',(3.53581482198805,-0.0146574021557552,
1.8325086226628));
#15411=CARTESIAN_POINT('Ctrl Pts',(3.63054607781447,-1.3251033111666,1.1131477025114));
#15412=CARTESIAN_POINT('Ctrl Pts',(3.68858906195055,-1.55236934417881,0.298485712909523));
#15413=CARTESIAN_POINT('Ctrl Pts',(3.7099437743963,-1.55362687475922,-0.000652149380348192));
#15414=CARTESIAN_POINT('',(3.746,-0.947228644581641,1.23383067917929));
#15415=CARTESIAN_POINT('Origin',(3.746,0.,0.));
#15416=CARTESIAN_POINT('Ctrl Pts',(3.1480562256037,-1.55328054787896,-0.000526513748883416));
#15417=CARTESIAN_POINT('Ctrl Pts',(3.16392945861747,-1.55399038993147,-0.222903896360382));
#15418=CARTESIAN_POINT('Ctrl Pts',(3.21649096332156,-1.40604281565034,-0.958389511212442));
#15419=CARTESIAN_POINT('Ctrl Pts',(3.30574073971599,-0.283353499784069,
-1.81052838148212));
#15420=CARTESIAN_POINT('Ctrl Pts',(3.41580555478699,1.35479857128691,-1.23328473077121));
#15421=CARTESIAN_POINT('Ctrl Pts',(3.525870369858,1.77698226704399,0.452636866150692));
#15422=CARTESIAN_POINT('Ctrl Pts',(3.635935184929,0.596883679625912,1.73212294945));
#15423=CARTESIAN_POINT('Ctrl Pts',(3.70931172830967,-0.540911968892668,
1.54576553416264));
#15424=CARTESIAN_POINT('Ctrl Pts',(3.746,-0.947228644581658,1.23383067917928));
#15425=CARTESIAN_POINT('Origin',(-0.840056225603703,0.,0.));
#15426=CARTESIAN_POINT('',(2.3099437743963,-1.55688307389266,-0.00107097220715865));
#15427=CARTESIAN_POINT('',(2.4480562256037,-1.55588265395775,0.00132172678777145));
#15428=CARTESIAN_POINT('',(-0.840056225603703,-1.5555,-7.61108830709034E-15));
#15429=CARTESIAN_POINT('Ctrl Pts',(2.3099437743963,-1.55688307389266,-0.00107097220715882));
#15430=CARTESIAN_POINT('Ctrl Pts',(2.31499646833321,-1.55743940426441,-0.0714352219473509));
#15431=CARTESIAN_POINT('Ctrl Pts',(2.35673743396045,-1.52137003123898,-0.652150212445693));
#15432=CARTESIAN_POINT('Ctrl Pts',(2.43516667127804,-0.791822273096899,
-1.65268520044665));
#15433=CARTESIAN_POINT('Ctrl Pts',(2.54523148634904,0.943989600391651,-1.57074361659946));
#15434=CARTESIAN_POINT('Ctrl Pts',(2.65529630142005,1.83098404786343,-0.0764251256222896));
#15435=CARTESIAN_POINT('Ctrl Pts',(2.76536111649104,1.0716057390628,1.48661337691892));
#15436=CARTESIAN_POINT('Ctrl Pts',(2.87542593156205,-0.65134861415973,1.71292230769104));
#15437=CARTESIAN_POINT('Ctrl Pts',(2.95695348419713,-1.49373789267815,0.739678208438402));
#15438=CARTESIAN_POINT('Ctrl Pts',(3.00179276514188,-1.5566761836761,0.115085162164511));
#15439=CARTESIAN_POINT('Ctrl Pts',(3.0099437743963,-1.55566092590572,0.00134228745768327));
#15440=CARTESIAN_POINT('Ctrl Pts',(2.4480562256037,-1.55588265395775,0.0013217267877714));
#15441=CARTESIAN_POINT('Ctrl Pts',(2.4771331618088,-1.55225867351481,-0.404282220158654));
#15442=CARTESIAN_POINT('Ctrl Pts',(2.54289836970422,-1.183940345012,-1.32750035240754));
#15443=CARTESIAN_POINT('Ctrl Pts',(2.64535184928997,0.36430880065416,-1.79600600778423));
#15444=CARTESIAN_POINT('Ctrl Pts',(2.75541666436099,1.69997652125137,-0.684386685169734));
#15445=CARTESIAN_POINT('Ctrl Pts',(2.86548147943198,1.50710917998158,1.04261238391286));
#15446=CARTESIAN_POINT('Ctrl Pts',(2.97554629450299,-0.0410030018867827,
1.83212804734855));
#15447=CARTESIAN_POINT('Ctrl Pts',(3.06973787656023,-1.33415753850242,1.09794221077487));
#15448=CARTESIAN_POINT('Ctrl Pts',(3.12724118692713,-1.55234971105672,0.291083507715543));
#15449=CARTESIAN_POINT('Ctrl Pts',(3.1480562256037,-1.55328054787896,-0.000526513748883416));
#15450=CARTESIAN_POINT('Origin',(-0.840056225603703,0.,0.));
#15451=CARTESIAN_POINT('',(1.6099437743963,-1.55305795606678,-1.80850188541769E-5));
#15452=CARTESIAN_POINT('',(1.7480562256037,-1.55668462553696,-0.00114432616101223));
#15453=CARTESIAN_POINT('',(-0.840056225603703,-1.5555,-7.61108830709034E-15));
#15454=CARTESIAN_POINT('Ctrl Pts',(1.6099437743963,-1.55305795606678,-1.80850188541068E-5));
#15455=CARTESIAN_POINT('Ctrl Pts',(1.62820017152454,-1.55308704590337,-0.255860187662811));
#15456=CARTESIAN_POINT('Ctrl Pts',(1.68314484034311,-1.37297545271786,-1.02580809014116));
#15457=CARTESIAN_POINT('Ctrl Pts',(1.77477778085203,-0.166990185543427,
-1.82495415320191));
#15458=CARTESIAN_POINT('Ctrl Pts',(1.88484259592303,1.43173046151262,-1.14389674372839));
#15459=CARTESIAN_POINT('Ctrl Pts',(1.99490741099403,1.74307212557223,0.565730014230139));
#15460=CARTESIAN_POINT('Ctrl Pts',(2.10497222606503,0.487082719346801,1.76666343036964));
#15461=CARTESIAN_POINT('Ctrl Pts',(2.20998434719912,-1.12911652195273,1.39684790771125));
#15462=CARTESIAN_POINT('Ctrl Pts',(2.27830819664287,-1.55339981665366,0.439488800759608));
#15463=CARTESIAN_POINT('Ctrl Pts',(2.3099437743963,-1.55688307389266,-0.00107097220715882));
#15464=CARTESIAN_POINT('Ctrl Pts',(1.7480562256037,-1.55668462553696,-0.00114432616101215));
#15465=CARTESIAN_POINT('Ctrl Pts',(1.75364859330979,-1.55732918071895,-0.0790501070845528));
#15466=CARTESIAN_POINT('Ctrl Pts',(1.79592923270621,-1.51685231829982,-0.667378849545193));
#15467=CARTESIAN_POINT('Ctrl Pts',(1.87489814379297,-0.767721750635221,
-1.66401720492241));
#15468=CARTESIAN_POINT('Ctrl Pts',(1.98496295886397,0.966714864421041,-1.55686024551378));
#15469=CARTESIAN_POINT('Ctrl Pts',(2.09502777393497,1.83190310060879,-0.0498093832135426));
#15470=CARTESIAN_POINT('Ctrl Pts',(2.20509258900597,1.04988649769768,1.50202859874456));
#15471=CARTESIAN_POINT('Ctrl Pts',(2.31515740407697,-0.676165934510966,
1.70327689450415));
#15472=CARTESIAN_POINT('Ctrl Pts',(2.39614528294288,-1.49885377405251,0.72441565460719));
#15473=CARTESIAN_POINT('Ctrl Pts',(2.44044489011846,-1.55683128660421,0.107494801301965));
#15474=CARTESIAN_POINT('Ctrl Pts',(2.4480562256037,-1.55588265395775,0.0013217267877714));
#15475=CARTESIAN_POINT('Origin',(-0.840056225603703,0.,0.));
#15476=CARTESIAN_POINT('',(0.909943774396297,-1.55680079221082,0.00119896459975423));
#15477=CARTESIAN_POINT('',(1.0480562256037,-1.55306103792732,0.000108654946547743));
#15478=CARTESIAN_POINT('',(-0.840056225603703,-1.5555,-7.61108830709034E-15));
#15479=CARTESIAN_POINT('Ctrl Pts',(0.909943774396297,-1.55680079221082,
0.0011989645997544));
#15480=CARTESIAN_POINT('Ctrl Pts',(0.941403874715868,-1.55327796540892,
-0.436951452674117));
#15481=CARTESIAN_POINT('Ctrl Pts',(1.00955224672577,-1.13303516878223,-1.39228499895859));
#15482=CARTESIAN_POINT('Ctrl Pts',(1.11438889042601,0.478745549796269,-1.76885677260357));
#15483=CARTESIAN_POINT('Ctrl Pts',(1.22445370549702,1.74037094585896,-0.574006059349687));
#15484=CARTESIAN_POINT('Ctrl Pts',(1.33451852056802,1.4371242290595,1.13714206962872));
#15485=CARTESIAN_POINT('Ctrl Pts',(1.44458333563902,-0.158367626905839,
1.82571195327325));
#15486=CARTESIAN_POINT('Ctrl Pts',(1.53639175358178,-1.37042853583496,1.03076565848081));
#15487=CARTESIAN_POINT('Ctrl Pts',(1.5915118998342,-1.55302858662355,0.258283129098596));
#15488=CARTESIAN_POINT('Ctrl Pts',(1.6099437743963,-1.55305795606678,-1.80850188541068E-5));
#15489=CARTESIAN_POINT('Ctrl Pts',(1.0480562256037,-1.55306103792732,0.00010865494654776));
#15490=CARTESIAN_POINT('Ctrl Pts',(1.06685229650112,-1.55290939488932,-0.263298122304044));
#15491=CARTESIAN_POINT('Ctrl Pts',(1.12233663908887,-1.36509992687415,-1.04106360824864));
#15492=CARTESIAN_POINT('Ctrl Pts',(1.21450925336695,-0.140448663256852,
-1.82717801011092));
#15493=CARTESIAN_POINT('Ctrl Pts',(1.32457406843795,1.4482001648677,-1.12297585223739));
#15494=CARTESIAN_POINT('Ctrl Pts',(1.43463888350896,1.73466831809981,0.591003114939824));
#15495=CARTESIAN_POINT('Ctrl Pts',(1.54470369857996,0.461357912009977,1.77355377153154));
#15496=CARTESIAN_POINT('Ctrl Pts',(1.64917614594488,-1.14101833937308,1.38231417461337));
#15497=CARTESIAN_POINT('Ctrl Pts',(1.71696032161946,-1.55310062907875,0.432044407258565));
#15498=CARTESIAN_POINT('Ctrl Pts',(1.7480562256037,-1.55668462553696,-0.00114432616101215));
#15499=CARTESIAN_POINT('Origin',(3.746,2.59090492670967E-16,0.));
#15500=CARTESIAN_POINT('',(3.746,1.42596824066806,-1.33593808861266));
#15501=CARTESIAN_POINT('Ctrl Pts',(3.746,-1.47669774220803,-0.496045317568157));
#15502=CARTESIAN_POINT('Ctrl Pts',(3.746,-1.46767695685173,-0.541988808072643));
#15503=CARTESIAN_POINT('Ctrl Pts',(3.746,-1.45648644230582,-0.587389991070906));
#15504=CARTESIAN_POINT('Ctrl Pts',(3.746,-1.44311389873171,-0.632094361836819));
#15505=CARTESIAN_POINT('Ctrl Pts',(3.746,-1.42605782020177,-0.689112778280139));
#15506=CARTESIAN_POINT('Ctrl Pts',(3.746,-1.40545429196885,-0.744998389936387));
#15507=CARTESIAN_POINT('Ctrl Pts',(3.746,-1.38158419381388,-0.799585222171636));
#15508=CARTESIAN_POINT('Ctrl Pts',(3.746,-1.37368982492332,-0.817638293735676));
#15509=CARTESIAN_POINT('Ctrl Pts',(3.746,-1.36543774335364,-0.835549283520522));
#15510=CARTESIAN_POINT('Ctrl Pts',(3.746,-1.35683689466255,-0.853312047813334));
#15511=CARTESIAN_POINT('Ctrl Pts',(3.746,-1.35082910092434,-0.865719547110724));
#15512=CARTESIAN_POINT('Ctrl Pts',(3.746,-1.34465035509199,-0.878056205693144));
#15513=CARTESIAN_POINT('Ctrl Pts',(3.746,-1.33830595790412,-0.890315239315174));
#15514=CARTESIAN_POINT('Ctrl Pts',(3.746,-1.30979394486407,-0.945407900783096));
#15515=CARTESIAN_POINT('Ctrl Pts',(3.746,-1.27801858921512,-0.998784714934468));
#15516=CARTESIAN_POINT('Ctrl Pts',(3.746,-1.24329464671849,-1.05026739307564));
#15517=CARTESIAN_POINT('Ctrl Pts',(3.746,-1.21549197477731,-1.09148840394304));
#15518=CARTESIAN_POINT('Ctrl Pts',(3.746,-1.1857977693504,-1.13149528660234));
#15519=CARTESIAN_POINT('Ctrl Pts',(3.746,-1.15434993371631,-1.17019219952651));
#15520=CARTESIAN_POINT('Ctrl Pts',(3.746,-1.13719225263809,-1.19130491769222));
#15521=CARTESIAN_POINT('Ctrl Pts',(3.746,-1.11951222068639,-1.21202760312318));
#15522=CARTESIAN_POINT('Ctrl Pts',(3.746,-1.10132992050009,-1.23234376607124));
#15523=CARTESIAN_POINT('Ctrl Pts',(3.746,-1.09329393703457,-1.24132284725793));
#15524=CARTESIAN_POINT('Ctrl Pts',(3.746,-1.08516036012286,-1.25022177347855));
#15525=CARTESIAN_POINT('Ctrl Pts',(3.746,-1.07694000121619,-1.25902972511263));
#15526=CARTESIAN_POINT('Ctrl Pts',(3.746,-1.03283866198974,-1.30628343596823));
#15527=CARTESIAN_POINT('Ctrl Pts',(3.746,-0.986178549327218,-1.35099330214769));
#15528=CARTESIAN_POINT('Ctrl Pts',(3.746,-0.937274426077663,-1.39297381895804));
#15529=CARTESIAN_POINT('Ctrl Pts',(3.746,-0.88731744035443,-1.43585813912562));
#15530=CARTESIAN_POINT('Ctrl Pts',(3.746,-0.835018254132845,-1.47589526383444));
#15531=CARTESIAN_POINT('Ctrl Pts',(3.746,-0.780662569084495,-1.51286704790872));
#15532=CARTESIAN_POINT('Ctrl Pts',(3.746,-0.7436636018178,-1.53803309682409));
#15533=CARTESIAN_POINT('Ctrl Pts',(3.746,-0.705710755964256,-1.56177845813373));
#15534=CARTESIAN_POINT('Ctrl Pts',(3.746,-0.666883407901705,-1.58402563062414));
#15535=CARTESIAN_POINT('Ctrl Pts',(3.746,-0.645022282612557,-1.59655154983858));
#15536=CARTESIAN_POINT('Ctrl Pts',(3.746,-0.622883789925495,-1.6086023884738));
#15537=CARTESIAN_POINT('Ctrl Pts',(3.746,-0.600481117989749,-1.62016304189199));
#15538=CARTESIAN_POINT('Ctrl Pts',(3.746,-0.590196075220556,-1.62547052553442));
#15539=CARTESIAN_POINT('Ctrl Pts',(3.746,-0.579853601557955,-1.63067552933902));
#15540=CARTESIAN_POINT('Ctrl Pts',(3.746,-0.569460455658503,-1.63577381540665));
#15541=CARTESIAN_POINT('Ctrl Pts',(3.746,-0.508562938414991,-1.66564667264543));
#15542=CARTESIAN_POINT('Ctrl Pts',(3.746,-0.446154194198239,-1.69174917719426));
#15543=CARTESIAN_POINT('Ctrl Pts',(3.746,-0.382545387994772,-1.71386835327625));
#15544=CARTESIAN_POINT('Ctrl Pts',(3.746,-0.35466355323937,-1.72356391666209));
#15545=CARTESIAN_POINT('Ctrl Pts',(3.746,-0.326550579846396,-1.73249376115586));
#15546=CARTESIAN_POINT('Ctrl Pts',(3.746,-0.298230303151154,-1.74063786866498));
#15547=CARTESIAN_POINT('Ctrl Pts',(3.746,-0.235797117155308,-1.75859188035626));
#15548=CARTESIAN_POINT('Ctrl Pts',(3.746,-0.172357953747863,-1.77273055536692));
#15549=CARTESIAN_POINT('Ctrl Pts',(3.746,-0.108199968151964,-1.78319103686655));
#15550=CARTESIAN_POINT('Ctrl Pts',(3.746,-0.0745450275340682,-1.78867822416575));
#15551=CARTESIAN_POINT('Ctrl Pts',(3.746,-0.0406918803384018,-1.79315250709968));
#15552=CARTESIAN_POINT('Ctrl Pts',(3.746,-0.00667991656329378,-1.79662849654071));
#15553=CARTESIAN_POINT('Ctrl Pts',(3.746,0.0113280635103416,-1.79846889449609));
#15554=CARTESIAN_POINT('Ctrl Pts',(3.746,0.02938058296973,-1.80002938298957));
#15555=CARTESIAN_POINT('Ctrl Pts',(3.746,0.0474718931605801,-1.8013117281377));
#15556=CARTESIAN_POINT('Ctrl Pts',(3.746,0.0588526815596273,-1.80211841923035));
#15557=CARTESIAN_POINT('Ctrl Pts',(3.746,0.0702488219832869,-1.80281503367119));
#15558=CARTESIAN_POINT('Ctrl Pts',(3.746,0.0816588921433358,-1.80340195481207));
#15559=CARTESIAN_POINT('Ctrl Pts',(3.746,0.0929006830918067,-1.80398021986009));
#15560=CARTESIAN_POINT('Ctrl Pts',(3.746,0.104146803429052,-1.80445151859496));
#15561=CARTESIAN_POINT('Ctrl Pts',(3.746,0.115393905881569,-1.80481667057579));
#15562=CARTESIAN_POINT('Ctrl Pts',(3.746,0.183216213581067,-1.8070186110405));
#15563=CARTESIAN_POINT('Ctrl Pts',(3.746,0.251093954109709,-1.80536580748111));
#15564=CARTESIAN_POINT('Ctrl Pts',(3.746,0.318708653135867,-1.80002989300725));
#15565=CARTESIAN_POINT('Ctrl Pts',(3.746,0.387721529400568,-1.79458363929841));
#15566=CARTESIAN_POINT('Ctrl Pts',(3.746,0.456461268077058,-1.78530046409679));
#15567=CARTESIAN_POINT('Ctrl Pts',(3.746,0.524607649211818,-1.77231086825431));
#15568=CARTESIAN_POINT('Ctrl Pts',(3.746,0.593233643116481,-1.75922985191468));
#15569=CARTESIAN_POINT('Ctrl Pts',(3.746,0.661258933134227,-1.74239002904673));
#15570=CARTESIAN_POINT('Ctrl Pts',(3.746,0.728360259383821,-1.72187222166165));
#15571=CARTESIAN_POINT('Ctrl Pts',(3.746,0.743398135805435,-1.71727403755495));
#15572=CARTESIAN_POINT('Ctrl Pts',(3.746,0.758389586060716,-1.71249092446917));
#15573=CARTESIAN_POINT('Ctrl Pts',(3.746,0.773330913555261,-1.70752343674532));
#15574=CARTESIAN_POINT('Ctrl Pts',(3.746,0.784683538833469,-1.70374907153422));
#15575=CARTESIAN_POINT('Ctrl Pts',(3.746,0.796007432279541,-1.6998680936069));
#15576=CARTESIAN_POINT('Ctrl Pts',(3.746,0.807286588730607,-1.69588605410984));
#15577=CARTESIAN_POINT('Ctrl Pts',(3.746,0.875332946409464,-1.67186268985525));
#15578=CARTESIAN_POINT('Ctrl Pts',(3.746,0.941879691186089,-1.6441232993263));
#15579=CARTESIAN_POINT('Ctrl Pts',(3.746,1.00658917108316,-1.61281865410435));
#15580=CARTESIAN_POINT('Ctrl Pts',(3.746,1.07146563013462,-1.58143322901528));
#15581=CARTESIAN_POINT('Ctrl Pts',(3.746,1.13449641889544,-1.54646400492537));
#15582=CARTESIAN_POINT('Ctrl Pts',(3.746,1.1953402412806,-1.50801070738774));
#15583=CARTESIAN_POINT('Ctrl Pts',(3.746,1.25490827911898,-1.47036370572122));
#15584=CARTESIAN_POINT('Ctrl Pts',(3.746,1.31238108813822,-1.42937691198823));
#15585=CARTESIAN_POINT('Ctrl Pts',(3.746,1.36742213546892,-1.38509732245781));
#15586=CARTESIAN_POINT('Ctrl Pts',(3.746,1.38725915006856,-1.36913878048634));
#15587=CARTESIAN_POINT('Ctrl Pts',(3.746,1.40678007373163,-1.35275210897049));
#15588=CARTESIAN_POINT('Ctrl Pts',(3.746,1.42596824066806,-1.33593808861266));
#15589=CARTESIAN_POINT('',(3.746,-1.954,-2.39295984553393E-16));
#15590=CARTESIAN_POINT('Origin',(3.746,0.,0.));
#15591=CARTESIAN_POINT('',(3.746,1.93026759572985,0.31272288043729));
#15592=CARTESIAN_POINT('Origin',(3.746,0.,0.));
#15593=CARTESIAN_POINT('Ctrl Pts',(3.746,1.93161712722296,0.313370286892444));
#15594=CARTESIAN_POINT('Ctrl Pts',(3.746,1.9170676653561,0.369522322556259));
#15595=CARTESIAN_POINT('Ctrl Pts',(3.746,1.8998959347821,0.424871136241905));
#15596=CARTESIAN_POINT('Ctrl Pts',(3.746,1.88004233230363,0.47924162453163));
#15597=CARTESIAN_POINT('Ctrl Pts',(3.746,1.85535918428823,0.546838163325029));
#15598=CARTESIAN_POINT('Ctrl Pts',(3.746,1.82653125128417,0.612923897257949));
#15599=CARTESIAN_POINT('Ctrl Pts',(3.746,1.79383671268108,0.677242695947379));
#15600=CARTESIAN_POINT('Ctrl Pts',(3.746,1.78248277438098,0.699578893461036));
#15601=CARTESIAN_POINT('Ctrl Pts',(3.746,1.7706621870656,0.721701691516324));
#15602=CARTESIAN_POINT('Ctrl Pts',(3.746,1.75838562059073,0.743599294082916));
#15603=CARTESIAN_POINT('Ctrl Pts',(3.746,1.75113290438732,0.75653589954795));
#15604=CARTESIAN_POINT('Ctrl Pts',(3.746,1.74372103488401,0.76939389653469));
#15605=CARTESIAN_POINT('Ctrl Pts',(3.746,1.73615214576412,0.782170750034265));
#15606=CARTESIAN_POINT('Ctrl Pts',(3.746,1.72916208156856,0.79397050357335));
#15607=CARTESIAN_POINT('Ctrl Pts',(3.746,1.7220428899102,0.80569294674123));
#15608=CARTESIAN_POINT('Ctrl Pts',(3.746,1.71479708222831,0.817335825950651));
#15609=CARTESIAN_POINT('Ctrl Pts',(3.746,1.67710478427548,0.877901451131049));
#15610=CARTESIAN_POINT('Ctrl Pts',(3.746,1.63598575516677,0.93632285307313));
#15611=CARTESIAN_POINT('Ctrl Pts',(3.746,1.59171677536116,0.992351466900363));
#15612=CARTESIAN_POINT('Ctrl Pts',(3.746,1.55959936474689,1.03300056259535));
#15613=CARTESIAN_POINT('Ctrl Pts',(3.746,1.52582301942198,1.07238952467534));
#15614=CARTESIAN_POINT('Ctrl Pts',(3.746,1.49048374238826,1.11040925249883));
#15615=CARTESIAN_POINT('Ctrl Pts',(3.746,1.47779773240559,1.12405748435845));
#15616=CARTESIAN_POINT('Ctrl Pts',(3.746,1.46491025583191,1.13752914647693));
#15617=CARTESIAN_POINT('Ctrl Pts',(3.746,1.451825579104,1.15081875907035));
#15618=CARTESIAN_POINT('Ctrl Pts',(3.746,1.44285839741738,1.15992638726385));
#15619=CARTESIAN_POINT('Ctrl Pts',(3.746,1.4337969487779,1.16895011253028));
#15620=CARTESIAN_POINT('Ctrl Pts',(3.746,1.42464791636957,1.17788291675216));
#15621=CARTESIAN_POINT('Ctrl Pts',(3.746,1.37477938008039,1.22657286030263));
#15622=CARTESIAN_POINT('Ctrl Pts',(3.746,1.3224413352858,1.27243994889247));
#15623=CARTESIAN_POINT('Ctrl Pts',(3.746,1.2678925715542,1.31525763541383));
#15624=CARTESIAN_POINT('Ctrl Pts',(3.746,1.21450160441821,1.35716651725668));
#15625=CARTESIAN_POINT('Ctrl Pts',(3.746,1.15899184088837,1.39615447094));
#15626=CARTESIAN_POINT('Ctrl Pts',(3.746,1.1015848969634,1.43196503344108));
#15627=CARTESIAN_POINT('Ctrl Pts',(3.746,1.06067163266189,1.45748680673574));
#15628=CARTESIAN_POINT('Ctrl Pts',(3.746,1.01879428835795,1.48139381167139));
#15629=CARTESIAN_POINT('Ctrl Pts',(3.746,0.976030100453615,1.50357741528629));
#15630=CARTESIAN_POINT('Ctrl Pts',(3.746,0.943715750416762,1.52034024342404));
#15631=CARTESIAN_POINT('Ctrl Pts',(3.746,0.910894959489004,1.53611876003808));
#15632=CARTESIAN_POINT('Ctrl Pts',(3.746,0.877600977094349,1.55086054046809));
#15633=CARTESIAN_POINT('Ctrl Pts',(3.746,0.866501124167434,1.5557752903083));
#15634=CARTESIAN_POINT('Ctrl Pts',(3.746,0.85534698976745,1.56057547136442));
#15635=CARTESIAN_POINT('Ctrl Pts',(3.746,0.844145132007207,1.56525679972139));
#15636=CARTESIAN_POINT('Ctrl Pts',(3.746,0.783860743145455,1.59045003329939));
#15637=CARTESIAN_POINT('Ctrl Pts',(3.746,0.722418897081141,1.61211276930956));
#15638=CARTESIAN_POINT('Ctrl Pts',(3.746,0.660025508652091,1.63001714294657));
#15639=CARTESIAN_POINT('Ctrl Pts',(3.746,0.630724724982861,1.63842528028099));
#15640=CARTESIAN_POINT('Ctrl Pts',(3.746,0.601213932081696,1.64600385046251));
#15641=CARTESIAN_POINT('Ctrl Pts',(3.746,0.571513967094748,1.65272527485204));
#15642=CARTESIAN_POINT('Ctrl Pts',(3.746,0.506895215101871,1.66734919969025));
#15643=CARTESIAN_POINT('Ctrl Pts',(3.746,0.441380137523852,1.67791885103208));
#15644=CARTESIAN_POINT('Ctrl Pts',(3.746,0.375309113523308,1.68451038836656));
#15645=CARTESIAN_POINT('Ctrl Pts',(3.746,0.343701084436922,1.68766374503));
#15646=CARTESIAN_POINT('Ctrl Pts',(3.746,0.311965969078073,1.68990590810348));
#15647=CARTESIAN_POINT('Ctrl Pts',(3.746,0.280142405068005,1.69124126858452));
#15648=CARTESIAN_POINT('Ctrl Pts',(3.746,0.260904293393882,1.69204852618934));
#15649=CARTESIAN_POINT('Ctrl Pts',(3.746,0.241633879772981,1.69252434567738));
#15650=CARTESIAN_POINT('Ctrl Pts',(3.746,0.222339944596673,1.69266927819294));
#15651=CARTESIAN_POINT('Ctrl Pts',(3.746,0.211331617752912,1.69275197073269));
#15652=CARTESIAN_POINT('Ctrl Pts',(3.746,0.200313308126325,1.69272690943876));
#15653=CARTESIAN_POINT('Ctrl Pts',(3.746,0.189294283975791,1.69259425622779));
#15654=CARTESIAN_POINT('Ctrl Pts',(3.746,0.124549117359031,1.69181481749266));
#15655=CARTESIAN_POINT('Ctrl Pts',(3.746,0.0599603848989907,1.68732902375792));
#15656=CARTESIAN_POINT('Ctrl Pts',(3.746,-0.00415842200663883,1.67924353111349));
#15657=CARTESIAN_POINT('Ctrl Pts',(3.746,-0.0682057305053929,1.67116705454204));
#15658=CARTESIAN_POINT('Ctrl Pts',(3.746,-0.131785198840776,1.65949843588597));
#15659=CARTESIAN_POINT('Ctrl Pts',(3.746,-0.194566709331386,1.64429548390334));
#15660=CARTESIAN_POINT('Ctrl Pts',(3.746,-0.256180836698767,1.62937522135313));
#15661=CARTESIAN_POINT('Ctrl Pts',(3.746,-0.317027247668399,1.6110503044156));
#15662=CARTESIAN_POINT('Ctrl Pts',(3.746,-0.376763100391235,1.58933625316552));
#15663=CARTESIAN_POINT('Ctrl Pts',(3.746,-0.39261189862501,1.58357519675779));
#15664=CARTESIAN_POINT('Ctrl Pts',(3.746,-0.408382314033138,1.57757538005586));
#15665=CARTESIAN_POINT('Ctrl Pts',(3.746,-0.424067457197251,1.57133669060524));
#15666=CARTESIAN_POINT('Ctrl Pts',(3.746,-0.43438249495729,1.5672339344759));
#15667=CARTESIAN_POINT('Ctrl Pts',(3.746,-0.444660866744379,1.563027674198));
#15668=CARTESIAN_POINT('Ctrl Pts',(3.746,-0.454886794556105,1.5587239402953));
#15669=CARTESIAN_POINT('Ctrl Pts',(3.746,-0.512125342014314,1.53463424576853));
#15670=CARTESIAN_POINT('Ctrl Pts',(3.746,-0.567832044889769,1.50745156624152));
#15671=CARTESIAN_POINT('Ctrl Pts',(3.746,-0.621711649124022,1.47723387270885));
#15672=CARTESIAN_POINT('Ctrl Pts',(3.746,-0.674641683099482,1.44754873362744));
#15673=CARTESIAN_POINT('Ctrl Pts',(3.746,-0.72580917835169,1.41493409040527));
#15674=CARTESIAN_POINT('Ctrl Pts',(3.746,-0.774899315695597,1.37940945108255));
#15675=CARTESIAN_POINT('Ctrl Pts',(3.746,-0.822419019818227,1.34502127372113));
#15676=CARTESIAN_POINT('Ctrl Pts',(3.746,-0.867992618095871,1.30790580816821));
#15677=CARTESIAN_POINT('Ctrl Pts',(3.746,-0.911293112387728,1.2680547652239));
#15678=CARTESIAN_POINT('Ctrl Pts',(3.746,-0.923453836159227,1.25686280233347));
#15679=CARTESIAN_POINT('Ctrl Pts',(3.746,-0.935434990894819,1.24545493657529));
#15680=CARTESIAN_POINT('Ctrl Pts',(3.746,-0.94722864458165,1.23383067917928));
#15681=CARTESIAN_POINT('Ctrl Pts',(0.223925917727934,-0.68582572912871,
1.39614588036676));
#15682=CARTESIAN_POINT('Ctrl Pts',(0.260614189418268,-1.14559493608735,
1.17029444461958));
#15683=CARTESIAN_POINT('Ctrl Pts',(0.333990732798937,-1.81718714798608,
0.233132812382442));
#15684=CARTESIAN_POINT('Ctrl Pts',(0.444055547869938,-1.19370785634296,
-1.39197976411031));
#15685=CARTESIAN_POINT('Ctrl Pts',(0.554120362940941,0.504597663383652,
-1.76120742504176));
#15686=CARTESIAN_POINT('Ctrl Pts',(0.664185178011943,1.74842530967382,-0.548918174671008));
#15687=CARTESIAN_POINT('Ctrl Pts',(0.774249993082944,1.42050197063444,1.15804372422));
#15688=CARTESIAN_POINT('Ctrl Pts',(0.884314808153947,-0.184910056920043,
1.82314603030263));
#15689=CARTESIAN_POINT('Ctrl Pts',(0.994379623224949,-1.62394765962336,
0.849216360445764));
#15690=CARTESIAN_POINT('Ctrl Pts',(1.10444443829595,-1.60282461854704,-0.888466040798839));
#15691=CARTESIAN_POINT('Ctrl Pts',(1.21450925336695,-0.140448663256852,
-1.82717801011092));
#15692=CARTESIAN_POINT('Ctrl Pts',(1.32457406843795,1.4482001648677,-1.12297585223739));
#15693=CARTESIAN_POINT('Ctrl Pts',(1.43463888350896,1.73466831809981,0.591003114939824));
#15694=CARTESIAN_POINT('Ctrl Pts',(1.54470369857996,0.461357912009977,1.77355377153154));
#15695=CARTESIAN_POINT('Ctrl Pts',(1.65476851365096,-1.22679288976659,1.36137127777947));
#15696=CARTESIAN_POINT('Ctrl Pts',(1.76483332872196,-1.81184045835624,-0.274928577921449));
#15697=CARTESIAN_POINT('Ctrl Pts',(1.87489814379297,-0.767721750635221,
-1.66401720492241));
#15698=CARTESIAN_POINT('Ctrl Pts',(1.98496295886397,0.966714864421041,-1.55686024551378));
#15699=CARTESIAN_POINT('Ctrl Pts',(2.09502777393497,1.83190310060879,-0.0498093832135426));
#15700=CARTESIAN_POINT('Ctrl Pts',(2.20509258900597,1.04988649769768,1.50202859874456));
#15701=CARTESIAN_POINT('Ctrl Pts',(2.31515740407697,-0.676165934510966,
1.70327689450415));
#15702=CARTESIAN_POINT('Ctrl Pts',(2.42522221914797,-1.79422194719185,0.372976819256964));
#15703=CARTESIAN_POINT('Ctrl Pts',(2.53528703421898,-1.29896077877424,-1.29269476323455));
#15704=CARTESIAN_POINT('Ctrl Pts',(2.64535184928997,0.36430880065416,-1.79600600778423));
#15705=CARTESIAN_POINT('Ctrl Pts',(2.75541666436099,1.69997652125137,-0.684386685169734));
#15706=CARTESIAN_POINT('Ctrl Pts',(2.86548147943198,1.50710917998158,1.04261238391286));
#15707=CARTESIAN_POINT('Ctrl Pts',(2.97554629450299,-0.0410030018867827,
1.83212804734855));
#15708=CARTESIAN_POINT('Ctrl Pts',(3.08561110957399,-1.55208086916726,0.974216686637734));
#15709=CARTESIAN_POINT('Ctrl Pts',(3.19567592464499,-1.66787900701797,-0.75965171870431));
#15710=CARTESIAN_POINT('Ctrl Pts',(3.30574073971599,-0.283353499784069,
-1.81052838148212));
#15711=CARTESIAN_POINT('Ctrl Pts',(3.41580555478699,1.35479857128691,-1.23328473077121));
#15712=CARTESIAN_POINT('Ctrl Pts',(3.525870369858,1.77698226704399,0.452636866150692));
#15713=CARTESIAN_POINT('Ctrl Pts',(3.635935184929,0.596883679625912,1.73212294945));
#15714=CARTESIAN_POINT('Ctrl Pts',(3.70931172830967,-0.540911968892668,
1.54576553416264));
#15715=CARTESIAN_POINT('Ctrl Pts',(3.746,-0.947228644581658,1.23383067917928));
#15716=CARTESIAN_POINT('Ctrl Pts',(0.30061727848529,-0.744392439309314,
1.51537102412036));
#15717=CARTESIAN_POINT('Ctrl Pts',(0.337305550175624,-1.24342405470534,
1.27023280017104));
#15718=CARTESIAN_POINT('Ctrl Pts',(0.410682093556292,-1.97236749267106,
0.253041400346528));
#15719=CARTESIAN_POINT('Ctrl Pts',(0.520746908627293,-1.29564562142443,
-1.51084913858754));
#15720=CARTESIAN_POINT('Ctrl Pts',(0.630811723698296,0.547688238516703,
-1.91160733051249));
#15721=CARTESIAN_POINT('Ctrl Pts',(0.740876538769298,1.89773367480937,-0.595793540064002));
#15722=CARTESIAN_POINT('Ctrl Pts',(0.850941353840301,1.54180702480734,1.25693591839158));
#15723=CARTESIAN_POINT('Ctrl Pts',(0.961006168911302,-0.200700618943537,
1.97883523914771));
#15724=CARTESIAN_POINT('Ctrl Pts',(1.0710709839823,-1.76262614293203,0.921735961782452));
#15725=CARTESIAN_POINT('Ctrl Pts',(1.18113579905331,-1.73969928060447,-0.964337404188605));
#15726=CARTESIAN_POINT('Ctrl Pts',(1.29120061412431,-0.152442404242143,
-1.98321153352872));
#15727=CARTESIAN_POINT('Ctrl Pts',(1.40126542919531,1.57187053145932,-1.21887339367457));
#15728=CARTESIAN_POINT('Ctrl Pts',(1.51133024426631,1.88280189246234,0.641472361977973));
#15729=CARTESIAN_POINT('Ctrl Pts',(1.62139505933731,0.500755989356165,1.92500800445885));
#15730=CARTESIAN_POINT('Ctrl Pts',(1.73145987440832,-1.33155598128528,1.47762681280468));
#15731=CARTESIAN_POINT('Ctrl Pts',(1.84152468947932,-1.96656421763085,-0.298406353192358));
#15732=CARTESIAN_POINT('Ctrl Pts',(1.95158950455032,-0.833282045851795,
-1.80611746339484));
#15733=CARTESIAN_POINT('Ctrl Pts',(2.06165431962132,1.04926835707545,-1.6898097382465));
#15734=CARTESIAN_POINT('Ctrl Pts',(2.17171913469233,1.9883401274153,-0.054062900670009));
#15735=CARTESIAN_POINT('Ctrl Pts',(2.28178394976332,1.13954250741214,1.63029569326931));
#15736=CARTESIAN_POINT('Ctrl Pts',(2.39184876483433,-0.733907737768787,
1.84872976977681));
#15737=CARTESIAN_POINT('Ctrl Pts',(2.50191357990533,-1.94744115772564,0.40482751302615));
#15738=CARTESIAN_POINT('Ctrl Pts',(2.61197839497634,-1.40988671263078,-1.40308560501082));
#15739=CARTESIAN_POINT('Ctrl Pts',(2.72204321004733,0.395419281112895,-1.94937756979045));
#15740=CARTESIAN_POINT('Ctrl Pts',(2.83210802511834,1.84514755815669,-0.742830506886256));
#15741=CARTESIAN_POINT('Ctrl Pts',(2.94217284018934,1.63581013534913,1.13164721408307));
#15742=CARTESIAN_POINT('Ctrl Pts',(3.05223765526034,-0.0445044904224903,
1.98858428368593));
#15743=CARTESIAN_POINT('Ctrl Pts',(3.16230247033134,-1.68462222272199,1.05741080420446));
#15744=CARTESIAN_POINT('Ctrl Pts',(3.27236728540234,-1.81030904758299,-0.824522866224651));
#15745=CARTESIAN_POINT('Ctrl Pts',(3.38243210047335,-0.307550728898814,
-1.96514009476201));
#15746=CARTESIAN_POINT('Ctrl Pts',(3.49249691554435,1.47049282407976,-1.33860219894057));
#15747=CARTESIAN_POINT('Ctrl Pts',(3.60256173061535,1.92872927945522,0.491290201875763));
#15748=CARTESIAN_POINT('Ctrl Pts',(3.71262654568635,0.647855102819084,1.88003915974805));
#15749=CARTESIAN_POINT('Ctrl Pts',(3.78600308906702,-0.587103637081617,
1.67776758395666));
#15750=CARTESIAN_POINT('Ctrl Pts',(3.82269136075736,-1.02811809381894,1.33919476910812));
#15751=CARTESIAN_POINT('Ctrl Pts',(0.377308639242645,-0.802959149489918,
1.63459616787395));
#15752=CARTESIAN_POINT('Ctrl Pts',(0.413996910932979,-1.34125317332332,
1.37017115572251));
#15753=CARTESIAN_POINT('Ctrl Pts',(0.487373454313647,-2.12754783735604,
0.272949988310614));
#15754=CARTESIAN_POINT('Ctrl Pts',(0.597438269384649,-1.3975833865059,-1.62971851306476));
#15755=CARTESIAN_POINT('Ctrl Pts',(0.707503084455652,0.590778813649754,
-2.06200723598321));
#15756=CARTESIAN_POINT('Ctrl Pts',(0.817567899526653,2.04704203994491,-0.642668905456995));
#15757=CARTESIAN_POINT('Ctrl Pts',(0.927632714597656,1.66311207898024,1.35582811256316));
#15758=CARTESIAN_POINT('Ctrl Pts',(1.03769752966866,-0.216491180967031,
2.1345244479928));
#15759=CARTESIAN_POINT('Ctrl Pts',(1.14776234473966,-1.9013046262407,0.994255563119137));
#15760=CARTESIAN_POINT('Ctrl Pts',(1.25782715981066,-1.87657394266189,-1.04020876757837));
#15761=CARTESIAN_POINT('Ctrl Pts',(1.36789197488167,-0.164436145227433,
-2.13924505694653));
#15762=CARTESIAN_POINT('Ctrl Pts',(1.47795678995266,1.69554089805093,-1.31477093511175));
#15763=CARTESIAN_POINT('Ctrl Pts',(1.58802160502367,2.03093546682488,0.69194160901612));
#15764=CARTESIAN_POINT('Ctrl Pts',(1.69808642009467,0.540154066702352,2.07646223738617));
#15765=CARTESIAN_POINT('Ctrl Pts',(1.80815123516567,-1.43631907280398,1.59388234782989));
#15766=CARTESIAN_POINT('Ctrl Pts',(1.91821605023667,-2.12128797690546,-0.321884128463266));
#15767=CARTESIAN_POINT('Ctrl Pts',(2.02828086530768,-0.898842341068367,
-1.94821772186726));
#15768=CARTESIAN_POINT('Ctrl Pts',(2.13834568037868,1.13182184972985,-1.82275923097922));
#15769=CARTESIAN_POINT('Ctrl Pts',(2.24841049544968,2.14477715422182,-0.0583164181264759));
#15770=CARTESIAN_POINT('Ctrl Pts',(2.35847531052068,1.2291985171266,1.75856278779405));
#15771=CARTESIAN_POINT('Ctrl Pts',(2.46854012559169,-0.791649541026606,
1.99418264504948));
#15772=CARTESIAN_POINT('Ctrl Pts',(2.57860494066269,-2.10066036825944,0.436678206795334));
#15773=CARTESIAN_POINT('Ctrl Pts',(2.68866975573369,-1.52081264648731,-1.51347644678709));
#15774=CARTESIAN_POINT('Ctrl Pts',(2.79873457080469,0.426529761571628,-2.10274913179667));
#15775=CARTESIAN_POINT('Ctrl Pts',(2.90879938587569,1.99031859506201,-0.801274328602775));
#15776=CARTESIAN_POINT('Ctrl Pts',(3.01886420094669,1.76451109071668,1.22068204425328));
#15777=CARTESIAN_POINT('Ctrl Pts',(3.1289290160177,-0.048005978958199,2.14504052002332));
#15778=CARTESIAN_POINT('Ctrl Pts',(3.2389938310887,-1.81716357627672,1.14060492177119));
#15779=CARTESIAN_POINT('Ctrl Pts',(3.3490586461597,-1.95273908814801,-0.88939401374499));
#15780=CARTESIAN_POINT('Ctrl Pts',(3.45912346123071,-0.331747958013558,
-2.11975180804191));
#15781=CARTESIAN_POINT('Ctrl Pts',(3.5691882763017,1.58618707687261,-1.44391966710993));
#15782=CARTESIAN_POINT('Ctrl Pts',(3.67925309137271,2.08047629186646,0.529943537600835));
#15783=CARTESIAN_POINT('Ctrl Pts',(3.78931790644371,0.698826526012254,2.02795537004609));
#15784=CARTESIAN_POINT('Ctrl Pts',(3.86269444982438,-0.633295305270564,
1.80976963375068));
#15785=CARTESIAN_POINT('Ctrl Pts',(3.89938272151471,-1.10900754305623,1.44455885903696));
#15786=CARTESIAN_POINT('Ctrl Pts',(0.454,-0.861525859670522,1.75382131162755));
#15787=CARTESIAN_POINT('Ctrl Pts',(0.490688271690334,-1.4390822919413,1.47010951127397));
#15788=CARTESIAN_POINT('Ctrl Pts',(0.564064815071003,-2.28272818204102,
0.292858576274699));
#15789=CARTESIAN_POINT('Ctrl Pts',(0.674129630142004,-1.49952115158736,
-1.74858788754198));
#15790=CARTESIAN_POINT('Ctrl Pts',(0.784194445213007,0.633869388782806,
-2.21240714145394));
#15791=CARTESIAN_POINT('Ctrl Pts',(0.894259260284009,2.19635040508046,-0.689544270849986));
#15792=CARTESIAN_POINT('Ctrl Pts',(1.00432407535501,1.78441713315314,1.45472030673473));
#15793=CARTESIAN_POINT('Ctrl Pts',(1.11438889042601,-0.232281742990522,
2.29021365683789));
#15794=CARTESIAN_POINT('Ctrl Pts',(1.22445370549701,-2.03998310954937,1.06677516445582));
#15795=CARTESIAN_POINT('Ctrl Pts',(1.33451852056802,-2.01344860471932,-1.11608013096813));
#15796=CARTESIAN_POINT('Ctrl Pts',(1.44458333563902,-0.176429886212727,
-2.29527858036434));
#15797=CARTESIAN_POINT('Ctrl Pts',(1.55464815071002,1.81921126464255,-1.41066847654893));
#15798=CARTESIAN_POINT('Ctrl Pts',(1.66471296578102,2.17906904118742,0.742410856054269));
#15799=CARTESIAN_POINT('Ctrl Pts',(1.77477778085202,0.579552144048537,2.22791647031348));
#15800=CARTESIAN_POINT('Ctrl Pts',(1.88484259592303,-1.54108216432267,1.71013788285509));
#15801=CARTESIAN_POINT('Ctrl Pts',(1.99490741099403,-2.27601173618007,-0.345361903734176));
#15802=CARTESIAN_POINT('Ctrl Pts',(2.10497222606503,-0.964402636284939,
-2.09031798033969));
#15803=CARTESIAN_POINT('Ctrl Pts',(2.21503704113604,1.21437534238426,-1.95570872371194));
#15804=CARTESIAN_POINT('Ctrl Pts',(2.32510185620703,2.30121418102833,-0.0625699355829409));
#15805=CARTESIAN_POINT('Ctrl Pts',(2.43516667127804,1.31885452684106,1.88682988231879));
#15806=CARTESIAN_POINT('Ctrl Pts',(2.54523148634904,-0.849391344284427,
2.13963552032215));
#15807=CARTESIAN_POINT('Ctrl Pts',(2.65529630142005,-2.25387957879323,0.468528900564519));
#15808=CARTESIAN_POINT('Ctrl Pts',(2.76536111649104,-1.63173858034385,-1.62386728856336));
#15809=CARTESIAN_POINT('Ctrl Pts',(2.87542593156205,0.457640242030363,-2.25612069380289));
#15810=CARTESIAN_POINT('Ctrl Pts',(2.98549074663305,2.13548963196732,-0.859718150319296));
#15811=CARTESIAN_POINT('Ctrl Pts',(3.09555556170405,1.89321204608423,1.30971687442349));
#15812=CARTESIAN_POINT('Ctrl Pts',(3.20562037677505,-0.0515074674939052,
2.3014967563607));
#15813=CARTESIAN_POINT('Ctrl Pts',(3.31568519184605,-1.94970492983146,1.22379903933792));
#15814=CARTESIAN_POINT('Ctrl Pts',(3.42575000691705,-2.09516912871303,-0.95426516126533));
#15815=CARTESIAN_POINT('Ctrl Pts',(3.53581482198806,-0.355945187128305,
-2.2743635213218));
#15816=CARTESIAN_POINT('Ctrl Pts',(3.64587963705906,1.70188132966546,-1.54923713527929));
#15817=CARTESIAN_POINT('Ctrl Pts',(3.75594445213006,2.23222330427769,0.568596873325905));
#15818=CARTESIAN_POINT('Ctrl Pts',(3.86600926720106,0.749797949205426,2.17587158034414));
#15819=CARTESIAN_POINT('Ctrl Pts',(3.93938581058173,-0.679486973459512,
1.94177168354471));
#15820=CARTESIAN_POINT('Ctrl Pts',(3.97607408227207,-1.18989699229351,1.5499229489658));
#15821=CARTESIAN_POINT('Ctrl Pts',(3.37813030787577,-1.95121195149822,-0.0006614001062776));
#15822=CARTESIAN_POINT('Ctrl Pts',(3.39400354088953,-1.95210364636843,-0.280009137568746));
#15823=CARTESIAN_POINT('Ctrl Pts',(3.40987677390329,-1.89597817583308,-0.559023351935746));
#15824=CARTESIAN_POINT('Ctrl Pts',(3.42575000691705,-1.78105443863531,-0.811270854507534));
#15825=CARTESIAN_POINT('Ctrl Pts',(3.46243827860739,-1.51542781485145,-1.39429794795082));
#15826=CARTESIAN_POINT('Ctrl Pts',(3.49912655029773,-0.935686500989876,
-1.83433073463632));
#15827=CARTESIAN_POINT('Ctrl Pts',(3.53581482198806,-0.302844757926788,
-1.93349273030531));
#15828=CARTESIAN_POINT('Ctrl Pts',(3.5725030936784,0.329996985136287,-2.0326547259743));
#15829=CARTESIAN_POINT('Ctrl Pts',(3.60919136536873,1.01593915740087,-1.79094593062679));
#15830=CARTESIAN_POINT('Ctrl Pts',(3.64587963705906,1.4473005726352,-1.31711919818552));
#15831=CARTESIAN_POINT('Ctrl Pts',(3.67925309137271,1.83968810741749,-0.886103124678848));
#15832=CARTESIAN_POINT('Ctrl Pts',(3.71262654568635,2.02141985840415,-0.263018386824143));
#15833=CARTESIAN_POINT('Ctrl Pts',(3.746,1.93161712722296,0.313370286892444));
#15834=CARTESIAN_POINT('',(0.454,-0.903606778650207,-1.26612599672284));
#15835=CARTESIAN_POINT('Ctrl Pts',(0.454,-0.905483447595497,-1.26759470319303));
#15836=CARTESIAN_POINT('Ctrl Pts',(0.454,-0.946792996117872,-1.24555610748147));
#15837=CARTESIAN_POINT('Ctrl Pts',(0.454,-0.986950518103967,-1.22160057893693));
#15838=CARTESIAN_POINT('Ctrl Pts',(0.454,-1.02580464664965,-1.19576145398998));
#15839=CARTESIAN_POINT('Ctrl Pts',(0.454,-1.07536139387572,-1.16280477650245));
#15840=CARTESIAN_POINT('Ctrl Pts',(0.454,-1.12279917616985,-1.12678580943023));
#15841=CARTESIAN_POINT('Ctrl Pts',(0.453999999999999,-1.16804123571681,
-1.08802164444088));
#15842=CARTESIAN_POINT('Ctrl Pts',(0.453999999999999,-1.18300393391255,
-1.07520135050746));
#15843=CARTESIAN_POINT('Ctrl Pts',(0.454,-1.19772631758119,-1.06208038985825));
#15844=CARTESIAN_POINT('Ctrl Pts',(0.454,-1.2122051216726,-1.0486691119922));
#15845=CARTESIAN_POINT('Ctrl Pts',(0.454,-1.22231850700918,-1.03930138935026));
#15846=CARTESIAN_POINT('Ctrl Pts',(0.453999999999999,-1.23231423927351,
-1.02979084142708));
#15847=CARTESIAN_POINT('Ctrl Pts',(0.453999999999999,-1.24218737666825,
-1.02014451854826));
#15848=CARTESIAN_POINT('Ctrl Pts',(0.453999999999999,-1.28655826323154,
-0.976792959555769));
#15849=CARTESIAN_POINT('Ctrl Pts',(0.454,-1.32833546524355,-0.9308210295969));
#15850=CARTESIAN_POINT('Ctrl Pts',(0.454,-1.3674403354694,-0.882581814883813));
#15851=CARTESIAN_POINT('Ctrl Pts',(0.454,-1.39875067745407,-0.843957819943645));
#15852=CARTESIAN_POINT('Ctrl Pts',(0.454,-1.42834763673987,-0.803879070882375));
#15853=CARTESIAN_POINT('Ctrl Pts',(0.454,-1.45617979978502,-0.762505438595754));
#15854=CARTESIAN_POINT('Ctrl Pts',(0.454,-1.47136486573799,-0.73993222594365));
#15855=CARTESIAN_POINT('Ctrl Pts',(0.454,-1.48602440875415,-0.716973256869188));
#15856=CARTESIAN_POINT('Ctrl Pts',(0.454,-1.50014851923412,-0.693652552625721));
#15857=CARTESIAN_POINT('Ctrl Pts',(0.454,-1.50639086297558,-0.683345648528146));
#15858=CARTESIAN_POINT('Ctrl Pts',(0.454,-1.51252805609302,-0.672968799088347));
#15859=CARTESIAN_POINT('Ctrl Pts',(0.454,-1.51855290632997,-0.66253550249243));
#15860=CARTESIAN_POINT('Ctrl Pts',(0.454,-1.55087574256289,-0.606561706634213));
#15861=CARTESIAN_POINT('Ctrl Pts',(0.454,-1.58001862028287,-0.548883105316666));
#15862=CARTESIAN_POINT('Ctrl Pts',(0.454,-1.60589599259671,-0.489854897524755));
#15863=CARTESIAN_POINT('Ctrl Pts',(0.454,-1.63233046396166,-0.429555905429438));
#15864=CARTESIAN_POINT('Ctrl Pts',(0.454,-1.65535805931995,-0.367847793451561));
#15865=CARTESIAN_POINT('Ctrl Pts',(0.454,-1.67485353015918,-0.305067491734872));
#15866=CARTESIAN_POINT('Ctrl Pts',(0.454,-1.68812373993677,-0.262334090702869));
#15867=CARTESIAN_POINT('Ctrl Pts',(0.454,-1.69975670599144,-0.219103041221796));
#15868=CARTESIAN_POINT('Ctrl Pts',(0.454,-1.70970147254438,-0.175472883179375));
#15869=CARTESIAN_POINT('Ctrl Pts',(0.454,-1.71530078814148,-0.150907296533324));
#15870=CARTESIAN_POINT('Ctrl Pts',(0.454,-1.72036473894179,-0.12621509073321));
#15871=CARTESIAN_POINT('Ctrl Pts',(0.454,-1.72488272738576,-0.101413288871812));
#15872=CARTESIAN_POINT('Ctrl Pts',(0.454,-1.72695692636838,-0.0900268338540925));
#15873=CARTESIAN_POINT('Ctrl Pts',(0.454,-1.72891634281505,-0.0786153607655636));
#15874=CARTESIAN_POINT('Ctrl Pts',(0.454,-1.73075889574632,-0.0671865737445383));
#15875=CARTESIAN_POINT('Ctrl Pts',(0.454,-1.74155503622729,-0.000221447200933339));
#15876=CARTESIAN_POINT('Ctrl Pts',(0.454,-1.74830390754617,0.0670885593810468));
#15877=CARTESIAN_POINT('Ctrl Pts',(0.454,-1.75089263790026,0.134383670605557));
#15878=CARTESIAN_POINT('Ctrl Pts',(0.454,-1.75202734170458,0.163880763108201));
#15879=CARTESIAN_POINT('Ctrl Pts',(0.454,-1.75236223751259,0.193375422393782));
#15880=CARTESIAN_POINT('Ctrl Pts',(0.454,-1.75188513727174,0.222839010041275));
#15881=CARTESIAN_POINT('Ctrl Pts',(0.454,-1.75083332989114,0.287793953035042));
#15882=CARTESIAN_POINT('Ctrl Pts',(0.454,-1.74583870802757,0.352597407685611));
#15883=CARTESIAN_POINT('Ctrl Pts',(0.454,-1.73711625989873,0.417014750824874));
#15884=CARTESIAN_POINT('Ctrl Pts',(0.454,-1.73254078339593,0.450805727343501));
#15885=CARTESIAN_POINT('Ctrl Pts',(0.454,-1.72693866052523,0.484490621676017));
#15886=CARTESIAN_POINT('Ctrl Pts',(0.454,-1.72033536334843,0.518036023454921));
#15887=CARTESIAN_POINT('Ctrl Pts',(0.454,-1.71683918324053,0.535796963674726));
#15888=CARTESIAN_POINT('Ctrl Pts',(0.454,-1.7130622836982,0.553518800658627));
#15889=CARTESIAN_POINT('Ctrl Pts',(0.454,-1.70900803188264,0.571196551544545));
#15890=CARTESIAN_POINT('Ctrl Pts',(0.454,-1.70645760125952,0.582317192111172));
#15891=CARTESIAN_POINT('Ctrl Pts',(0.454,-1.70379740670489,0.59342038571861));
#15892=CARTESIAN_POINT('Ctrl Pts',(0.454,-1.70102823002613,0.604504883893459));
#15893=CARTESIAN_POINT('Ctrl Pts',(0.454,-1.69829989761203,0.615425890088691));
#15894=CARTESIAN_POINT('Ctrl Pts',(0.454,-1.69546799387054,0.626319814603402));
#15895=CARTESIAN_POINT('Ctrl Pts',(0.454,-1.69253427969405,0.63718369519264));
#15896=CARTESIAN_POINT('Ctrl Pts',(0.454,-1.67484336232207,0.702695194364307));
#15897=CARTESIAN_POINT('Ctrl Pts',(0.454,-1.65344939464525,0.767134543862278));
#15898=CARTESIAN_POINT('Ctrl Pts',(0.454,-1.62860949461081,0.830247232310506));
#15899=CARTESIAN_POINT('Ctrl Pts',(0.454,-1.60325594047626,0.894665002145749));
#15900=CARTESIAN_POINT('Ctrl Pts',(0.454,-1.57431228886208,0.957701558306191));
#15901=CARTESIAN_POINT('Ctrl Pts',(0.454,-1.5419968261977,1.01908871346515));
#15902=CARTESIAN_POINT('Ctrl Pts',(0.454,-1.5094539404335,1.08090788648691));
#15903=CARTESIAN_POINT('Ctrl Pts',(0.454,-1.47349128606835,1.14105534222757));
#15904=CARTESIAN_POINT('Ctrl Pts',(0.454,-1.43428052126492,1.19924548512233));
#15905=CARTESIAN_POINT('Ctrl Pts',(0.454,-1.42549303760002,1.21228641744561));
#15906=CARTESIAN_POINT('Ctrl Pts',(0.454,-1.41654222718529,1.22522896377067));
#15907=CARTESIAN_POINT('Ctrl Pts',(0.454,-1.4074296992568,1.23806975015137));
#15908=CARTESIAN_POINT('Ctrl Pts',(0.454,-1.40050600488519,1.24782617351587));
#15909=CARTESIAN_POINT('Ctrl Pts',(0.454,-1.39348872939356,1.2575239974115));
#15910=CARTESIAN_POINT('Ctrl Pts',(0.454,-1.38638785362935,1.26714953450667));
#15911=CARTESIAN_POINT('Ctrl Pts',(0.454,-1.34354833476087,1.32522031221069));
#15912=CARTESIAN_POINT('Ctrl Pts',(0.454,-1.29759234685035,1.38077208883289));
#15913=CARTESIAN_POINT('Ctrl Pts',(0.454,-1.24876265241614,1.43352592094888));
#15914=CARTESIAN_POINT('Ctrl Pts',(0.454,-1.19980697925523,1.48641585591531));
#15915=CARTESIAN_POINT('Ctrl Pts',(0.454,-1.14796231910694,1.53649439668058));
#15916=CARTESIAN_POINT('Ctrl Pts',(0.454,-1.09342367488196,1.58346421475321));
#15917=CARTESIAN_POINT('Ctrl Pts',(0.454,-1.04002865799837,1.62944911710359));
#15918=CARTESIAN_POINT('Ctrl Pts',(0.454,-0.984050882431382,1.67245516047572));
#15919=CARTESIAN_POINT('Ctrl Pts',(0.454,-0.925633527523863,1.71217418185344));
#15920=CARTESIAN_POINT('Ctrl Pts',(0.454,-0.904579654827432,1.72648909256854));
#15921=CARTESIAN_POINT('Ctrl Pts',(0.454,-0.883208561787645,1.74037670661332));
#15922=CARTESIAN_POINT('Ctrl Pts',(0.454,-0.861525859670522,1.75382131162755));
#15923=CARTESIAN_POINT('Ctrl Pts',(0.454,-0.905483447595502,-1.26759470319303));
#15924=CARTESIAN_POINT('Ctrl Pts',(0.487373454313647,-0.525928763905175,
-1.53514395112967));
#15925=CARTESIAN_POINT('Ctrl Pts',(0.557435180317628,0.542057967958432,
-1.72469696100193));
#15926=CARTESIAN_POINT('Ctrl Pts',(0.664185178011943,1.74842530967382,-0.548918174671008));
#15927=CARTESIAN_POINT('Ctrl Pts',(0.774249993082944,1.42050197063444,1.15804372422));
#15928=CARTESIAN_POINT('Ctrl Pts',(0.884314808153947,-0.184910056920043,
1.82314603030263));
#15929=CARTESIAN_POINT('Ctrl Pts',(0.975583552327533,-1.37819925413147,
1.01553700625721));
#15930=CARTESIAN_POINT('Ctrl Pts',(1.03016402481079,-1.55320538871742,0.250848661967433));
#15931=CARTESIAN_POINT('Ctrl Pts',(1.0480562256037,-1.55306103792732,0.00010865494654776));
#15932=CARTESIAN_POINT('Origin',(0.454,-2.59090492670967E-16,0.));
#15933=CARTESIAN_POINT('',(0.454000000000001,-1.954,-2.39295984553393E-16));
#15934=CARTESIAN_POINT('Origin',(0.454000000000001,0.,0.));
#15935=CARTESIAN_POINT('Origin',(0.454000000000001,0.,0.));
#15936=CARTESIAN_POINT('',(0.454,0.903606778650208,-1.26612599672284));
#15937=CARTESIAN_POINT('Ctrl Pts',(0.454,0.863551653131346,1.75602537289062));
#15938=CARTESIAN_POINT('Ctrl Pts',(0.454,0.913011386895007,1.72571903943065));
#15939=CARTESIAN_POINT('Ctrl Pts',(0.454,0.960937458194194,1.69313908228652));
#15940=CARTESIAN_POINT('Ctrl Pts',(0.454,1.00714499237834,1.65827960401643));
#15941=CARTESIAN_POINT('Ctrl Pts',(0.454,1.0645928742677,1.61494028228584));
#15942=CARTESIAN_POINT('Ctrl Pts',(0.454,1.11938591595968,1.56807765715797));
#15943=CARTESIAN_POINT('Ctrl Pts',(0.454000000000001,1.17136033785776,1.51803256103724));
#15944=CARTESIAN_POINT('Ctrl Pts',(0.454000000000001,1.18940964604431,1.50065325540726));
#15945=CARTESIAN_POINT('Ctrl Pts',(0.454,1.20711863746561,1.48288991242546));
#15946=CARTESIAN_POINT('Ctrl Pts',(0.454,1.22447914419062,1.46475618062676));
#15947=CARTESIAN_POINT('Ctrl Pts',(0.454,1.23473533695067,1.45404318406898));
#15948=CARTESIAN_POINT('Ctrl Pts',(0.454,1.24486988911837,1.44320091040706));
#15949=CARTESIAN_POINT('Ctrl Pts',(0.454,1.25488099887649,1.43223214039003));
#15950=CARTESIAN_POINT('Ctrl Pts',(0.454,1.26412654056888,1.42210217248867));
#15951=CARTESIAN_POINT('Ctrl Pts',(0.454,1.27326044703626,1.41187126626082));
#15952=CARTESIAN_POINT('Ctrl Pts',(0.454,1.28228129577652,1.40154248174902));
#15953=CARTESIAN_POINT('Ctrl Pts',(0.454,1.32920718312896,1.34781279483776));
#15954=CARTESIAN_POINT('Ctrl Pts',(0.454,1.37308198830637,1.29143148746947));
#15955=CARTESIAN_POINT('Ctrl Pts',(0.454,1.41374875944775,1.23273584565278));
#15956=CARTESIAN_POINT('Ctrl Pts',(0.454,1.44325274809575,1.19015180218825));
#15957=CARTESIAN_POINT('Ctrl Pts',(0.454,1.47106724855506,1.14634889346906));
#15958=CARTESIAN_POINT('Ctrl Pts',(0.454,1.49711593321256,1.10145078924334));
#15959=CARTESIAN_POINT('Ctrl Pts',(0.454,1.50646681252166,1.08533340138511));
#15960=CARTESIAN_POINT('Ctrl Pts',(0.454,1.51559000541425,1.06907486083694));
#15961=CARTESIAN_POINT('Ctrl Pts',(0.454,1.52448151607123,1.05268084780668));
#15962=CARTESIAN_POINT('Ctrl Pts',(0.454,1.53057504708402,1.04144570108324));
#15963=CARTESIAN_POINT('Ctrl Pts',(0.454,1.53656081317822,1.03014488360131));
#15964=CARTESIAN_POINT('Ctrl Pts',(0.454,1.54243405273428,1.01878683589326));
#15965=CARTESIAN_POINT('Ctrl Pts',(0.454,1.57444727255085,0.956877616203873));
#15966=CARTESIAN_POINT('Ctrl Pts',(0.454,1.60303973510773,0.89343041122372));
#15967=CARTESIAN_POINT('Ctrl Pts',(0.454,1.6280702961961,0.828758872414623));
#15968=CARTESIAN_POINT('Ctrl Pts',(0.454,1.6525695670393,0.765460029870219));
#15969=CARTESIAN_POINT('Ctrl Pts',(0.454,1.6736566518802,0.700987273413124));
#15970=CARTESIAN_POINT('Ctrl Pts',(0.454,1.69115094315255,0.635627431361354));
#15971=CARTESIAN_POINT('Ctrl Pts',(0.454,1.70361893851176,0.58904616695378));
#15972=CARTESIAN_POINT('Ctrl Pts',(0.454,1.71426107355774,0.542014153906118));
#15973=CARTESIAN_POINT('Ctrl Pts',(0.454,1.72299599012096,0.49463697610565));
#15974=CARTESIAN_POINT('Ctrl Pts',(0.454,1.72959643622789,0.458836919344082));
#15975=CARTESIAN_POINT('Ctrl Pts',(0.454000000000001,1.73510760988993,0.422839796026985));
#15976=CARTESIAN_POINT('Ctrl Pts',(0.454000000000001,1.73948907456737,0.386692710613922));
#15977=CARTESIAN_POINT('Ctrl Pts',(0.454000000000001,1.7409498004039,0.374641721854365));
#15978=CARTESIAN_POINT('Ctrl Pts',(0.454,1.74228510356595,0.362572258504674));
#15979=CARTESIAN_POINT('Ctrl Pts',(0.454,1.74349280108337,0.350491842553832));
#15980=CARTESIAN_POINT('Ctrl Pts',(0.454,1.74999222909259,0.285479045341838));
#15981=CARTESIAN_POINT('Ctrl Pts',(0.454,1.75277705338185,0.220389744978822));
#15982=CARTESIAN_POINT('Ctrl Pts',(0.454,1.75168943631667,0.155487404454911));
#15983=CARTESIAN_POINT('Ctrl Pts',(0.454,1.7511786721516,0.125008120127728));
#15984=CARTESIAN_POINT('Ctrl Pts',(0.454,1.74981315196432,0.0945701230721414));
#15985=CARTESIAN_POINT('Ctrl Pts',(0.454,1.74757257969712,0.0642013941078475));
#15986=CARTESIAN_POINT('Ctrl Pts',(0.454,1.74269776618386,-0.0018718553483526));
#15987=CARTESIAN_POINT('Ctrl Pts',(0.454,1.73368359948819,-0.0676189542128947));
#15988=CARTESIAN_POINT('Ctrl Pts',(0.454,1.72070227983376,-0.132736582318621));
#15989=CARTESIAN_POINT('Ctrl Pts',(0.454,1.71449208835406,-0.163888495221565));
#15990=CARTESIAN_POINT('Ctrl Pts',(0.454,1.70737328909369,-0.194895983856983));
#15991=CARTESIAN_POINT('Ctrl Pts',(0.454,1.69936136020235,-0.225723375579589));
#15992=CARTESIAN_POINT('Ctrl Pts',(0.454,1.69451799574347,-0.244359124280579));
#15993=CARTESIAN_POINT('Ctrl Pts',(0.454000000000001,1.68934820366496,-0.262929023221881));
#15994=CARTESIAN_POINT('Ctrl Pts',(0.454000000000001,1.68385507404296,-0.281424835612363));
#15995=CARTESIAN_POINT('Ctrl Pts',(0.454000000000001,1.68072088746442,-0.29197789569699));
#15996=CARTESIAN_POINT('Ctrl Pts',(0.454,1.67748072537069,-0.30250905044186));
#15997=CARTESIAN_POINT('Ctrl Pts',(0.454,1.67413744771922,-0.31300948337107));
#15998=CARTESIAN_POINT('Ctrl Pts',(0.454,1.65449317315503,-0.374707436400236));
#15999=CARTESIAN_POINT('Ctrl Pts',(0.454,1.63134961131065,-0.435173893456361));
#16000=CARTESIAN_POINT('Ctrl Pts',(0.454,1.60490028261305,-0.494140152831118));
#16001=CARTESIAN_POINT('Ctrl Pts',(0.454000000000001,1.57848042422025,-0.553040710967983));
#16002=CARTESIAN_POINT('Ctrl Pts',(0.454,1.54876141221147,-0.610445269174527));
#16003=CARTESIAN_POINT('Ctrl Pts',(0.454,1.5158949004578,-0.666054964491294));
#16004=CARTESIAN_POINT('Ctrl Pts',(0.454,1.48363949654564,-0.720630673569242));
#16005=CARTESIAN_POINT('Ctrl Pts',(0.454000000000001,1.44835179261319,-0.773478294266712));
#16006=CARTESIAN_POINT('Ctrl Pts',(0.454000000000001,1.41014670969038,-0.824274448844553));
#16007=CARTESIAN_POINT('Ctrl Pts',(0.454000000000001,1.40001039673298,-0.837751339363897));
#16008=CARTESIAN_POINT('Ctrl Pts',(0.454000000000001,1.38966860276793,-0.851083569202111));
#16009=CARTESIAN_POINT('Ctrl Pts',(0.454000000000001,1.37912323125007,-0.864264516319142));
#16010=CARTESIAN_POINT('Ctrl Pts',(0.454000000000001,1.37218815669918,-0.872932854912353));
#16011=CARTESIAN_POINT('Ctrl Pts',(0.454000000000001,1.36516478597537,-0.881535910870752));
#16012=CARTESIAN_POINT('Ctrl Pts',(0.454000000000001,1.35806349294299,-0.89006035307576));
#16013=CARTESIAN_POINT('Ctrl Pts',(0.454,1.31831518441419,-0.937774502774395));
#16014=CARTESIAN_POINT('Ctrl Pts',(0.454000000000001,1.27605572448459,-0.983120693942016));
#16015=CARTESIAN_POINT('Ctrl Pts',(0.454000000000001,1.23142674553036,-1.02583345557658));
#16016=CARTESIAN_POINT('Ctrl Pts',(0.454000000000001,1.18758428349663,-1.06779347066542));
#16017=CARTESIAN_POINT('Ctrl Pts',(0.454,1.1414543704636,-1.10721259976975));
#16018=CARTESIAN_POINT('Ctrl Pts',(0.454000000000001,1.09314756187649,-1.14379543108553));
#16019=CARTESIAN_POINT('Ctrl Pts',(0.454000000000001,1.04638611087288,-1.1792079603786));
#16020=CARTESIAN_POINT('Ctrl Pts',(0.454000000000001,0.997584202053025,
-1.2119630573062));
#16021=CARTESIAN_POINT('Ctrl Pts',(0.454000000000001,0.946829359075407,
-1.24174554702703));
#16022=CARTESIAN_POINT('Ctrl Pts',(0.454000000000001,0.932575297379321,
-1.2501097034511));
#16023=CARTESIAN_POINT('Ctrl Pts',(0.454000000000001,0.918167154629348,
-1.25823909631819));
#16024=CARTESIAN_POINT('Ctrl Pts',(0.454000000000001,0.903606778650211,
-1.26612599672283));
#16025=CARTESIAN_POINT('Origin',(0.454,0.,0.));
#16026=CARTESIAN_POINT('Origin',(-0.840056225603703,0.,0.));
#16027=CARTESIAN_POINT('Ctrl Pts',(0.454,0.903606778650207,-1.26612599672284));
#16028=CARTESIAN_POINT('Ctrl Pts',(0.490688271690334,1.32055872730335,-0.9685563961068));
#16029=CARTESIAN_POINT('Ctrl Pts',(0.564064815071002,1.83091854106863,0.0652892855698468));
#16030=CARTESIAN_POINT('Ctrl Pts',(0.674129630142005,0.951615547993874,
1.56747461872394));
#16031=CARTESIAN_POINT('Ctrl Pts',(0.784194445213006,-0.784116518650487,
1.65578585359825));
#16032=CARTESIAN_POINT('Ctrl Pts',(0.862799159964437,-1.51990443805225,
0.6571547169837));
#16033=CARTESIAN_POINT('Ctrl Pts',(0.904715603025534,-1.55738623033857,
0.0740126379323188));
#16034=CARTESIAN_POINT('Ctrl Pts',(0.909943774396297,-1.55680079221082,
0.0011989645997544));
#16035=CARTESIAN_POINT('Ctrl Pts',(0.223925917727934,1.13509973994375,-1.5904919303095));
#16036=CARTESIAN_POINT('Ctrl Pts',(0.260614189418268,1.6588696580847,-1.21668865187572));
#16037=CARTESIAN_POINT('Ctrl Pts',(0.333990732798937,2.2999773894234,0.0820155988450519));
#16038=CARTESIAN_POINT('Ctrl Pts',(0.444055547869938,1.19540776649311,1.96904236900455));
#16039=CARTESIAN_POINT('Ctrl Pts',(0.554120362940941,-0.984997542554195,
2.07997785787913));
#16040=CARTESIAN_POINT('Ctrl Pts',(0.664185178011941,-2.27921456954046,
0.323431730109015));
#16041=CARTESIAN_POINT('Ctrl Pts',(0.774249993082947,-1.52427599397599,
-1.72538071835201));
#16042=CARTESIAN_POINT('Ctrl Pts',(0.884314808153945,0.601394281132697,
-2.22201615793466));
#16043=CARTESIAN_POINT('Ctrl Pts',(0.99437962322495,2.18623261215584,-0.721059363528956));
#16044=CARTESIAN_POINT('Ctrl Pts',(1.10444443829595,1.80529781008181,1.42846390488879));
#16045=CARTESIAN_POINT('Ctrl Pts',(1.21450925336695,-0.198939468321444,
2.29343693776659));
#16046=CARTESIAN_POINT('Ctrl Pts',(1.32457406843796,-2.0242846057989,1.09626001120675));
#16047=CARTESIAN_POINT('Ctrl Pts',(1.43463888350895,-2.02944435581129,-1.08667857505481));
#16048=CARTESIAN_POINT('Ctrl Pts',(1.54470369857996,-0.209771020605504,
-2.29248499862201));
#16049=CARTESIAN_POINT('Ctrl Pts',(1.65476851365096,1.79852222551955,-1.4369490435521));
#16050=CARTESIAN_POINT('Ctrl Pts',(1.76483332872197,2.18962580094384,0.710663097271417));
#16051=CARTESIAN_POINT('Ctrl Pts',(1.87489814379296,0.61186733114989,2.21926090835247));
#16052=CARTESIAN_POINT('Ctrl Pts',(1.98496295886397,-1.51606846270638,1.73235083706963));
#16053=CARTESIAN_POINT('Ctrl Pts',(2.09502777393497,-2.28078940850763,-0.312250355178937));
#16054=CARTESIAN_POINT('Ctrl Pts',(2.20509258900597,-0.994677416670744,
-2.07608285546304));
#16055=CARTESIAN_POINT('Ctrl Pts',(2.31515740407697,1.18582814475428,-1.97314884399573));
#16056=CARTESIAN_POINT('Ctrl Pts',(2.42522221914798,2.30005967825467,-0.0960043043818408));
#16057=CARTESIAN_POINT('Ctrl Pts',(2.53528703421898,1.34613797115314,1.86746546994507));
#16058=CARTESIAN_POINT('Ctrl Pts',(2.64535184928998,-0.818216131191326,
2.15175196993141));
#16059=CARTESIAN_POINT('Ctrl Pts',(2.75541666436098,-2.24681886682819,0.501233358060979));
#16060=CARTESIAN_POINT('Ctrl Pts',(2.86548147943199,-1.65519041947554,-1.59998562053935));
#16061=CARTESIAN_POINT('Ctrl Pts',(2.97554629450299,0.424857253226333,-2.26252866381124));
#16062=CARTESIAN_POINT('Ctrl Pts',(3.08561110957399,2.12267350101962,-0.890667219319853));
#16063=CARTESIAN_POINT('Ctrl Pts',(3.19567592464499,1.91223022331427,1.28208092650808));
#16064=CARTESIAN_POINT('Ctrl Pts',(3.30574073971599,-0.0184124486096701,
2.30197483039737));
#16065=CARTESIAN_POINT('Ctrl Pts',(3.41580555478699,-1.93103317110253,1.25205388869926));
#16066=CARTESIAN_POINT('Ctrl Pts',(3.525870369858,-2.11014175528073,-0.923812400732872));
#16067=CARTESIAN_POINT('Ctrl Pts',(3.635935184929,-0.3862086545477,-2.2688026413651));
#16068=CARTESIAN_POINT('Ctrl Pts',(3.70931172830967,0.986026251664791,-1.80552819117983));
#16069=CARTESIAN_POINT('Ctrl Pts',(3.746,1.42596824066807,-1.33593808861265));
#16070=CARTESIAN_POINT('Ctrl Pts',(0.30061727848529,1.05793541951257,-1.48236995244728));
#16071=CARTESIAN_POINT('Ctrl Pts',(0.337305550175624,1.54609934782425,-1.13397789995275));
#16072=CARTESIAN_POINT('Ctrl Pts',(0.410682093556291,2.14362443997181,0.0764401610866495));
#16073=CARTESIAN_POINT('Ctrl Pts',(0.520746908627294,1.11414369366003,1.83518645224435));
#16074=CARTESIAN_POINT('Ctrl Pts',(0.630811723698295,-0.918037201252959,
1.93858052311883));
#16075=CARTESIAN_POINT('Ctrl Pts',(0.740876538769298,-2.12427308097651,
0.301444772680075));
#16076=CARTESIAN_POINT('Ctrl Pts',(0.8509413538403,-1.4206553894725,-1.60808897214537));
#16077=CARTESIAN_POINT('Ctrl Pts',(0.961006168911301,0.56051137068722,-2.07096302949096));
#16078=CARTESIAN_POINT('Ctrl Pts',(1.0710709839823,2.03761205672355,-0.672041595469201));
#16079=CARTESIAN_POINT('Ctrl Pts',(1.18113579905331,1.68257328307437,1.33135662646876));
#16080=CARTESIAN_POINT('Ctrl Pts',(1.29120061412431,-0.185415521182909,
2.13752860960214));
#16081=CARTESIAN_POINT('Ctrl Pts',(1.40126542919531,-1.88667331009592,1.02173602375095));
#16082=CARTESIAN_POINT('Ctrl Pts',(1.51133024426631,-1.89148229921102,-1.0128059356554));
#16083=CARTESIAN_POINT('Ctrl Pts',(1.62139505933732,-0.195510742251477,
-2.13664138348197));
#16084=CARTESIAN_POINT('Ctrl Pts',(1.73145987440832,1.6762583041839,-1.33926494361086));
#16085=CARTESIAN_POINT('Ctrl Pts',(1.84152468947932,2.04077457581997,0.662352069590991));
#16086=CARTESIAN_POINT('Ctrl Pts',(1.95158950455032,0.570272460548859,2.0683950823582));
#16087=CARTESIAN_POINT('Ctrl Pts',(2.06165431962132,-1.41300580791476,1.61458526071817));
#16088=CARTESIAN_POINT('Ctrl Pts',(2.17171913469233,-2.12574086205756,-0.291023509982963));
#16089=CARTESIAN_POINT('Ctrl Pts',(2.28178394976333,-0.927059035479461,
-1.93495030379091));
#16090=CARTESIAN_POINT('Ctrl Pts',(2.39184876483433,1.1052152966334,-1.83901376819698));
#16091=CARTESIAN_POINT('Ctrl Pts',(2.50191357990533,2.14370113479092,-0.0894779114619904));
#16092=CARTESIAN_POINT('Ctrl Pts',(2.61197839497633,1.25462722712303,1.74051477226969));
#16093=CARTESIAN_POINT('Ctrl Pts',(2.72204321004734,-0.762593625514126,
2.00547541585129));
#16094=CARTESIAN_POINT('Ctrl Pts',(2.83210802511834,-2.09407964498735,0.467159408353149));
#16095=CARTESIAN_POINT('Ctrl Pts',(2.94217284018934,-1.54267022463401,-1.49121825960709));
#16096=CARTESIAN_POINT('Ctrl Pts',(3.05223765526034,0.395975367281145,-2.10872148664837));
#16097=CARTESIAN_POINT('Ctrl Pts',(3.16230247033134,1.97837370740714,-0.83011947334596));
#16098=CARTESIAN_POINT('Ctrl Pts',(3.27236728540235,1.78223640823567,1.19492479392305));
#16099=CARTESIAN_POINT('Ctrl Pts',(3.38243210047334,-0.017160766458366,
2.14548609448584));
#16100=CARTESIAN_POINT('Ctrl Pts',(3.49249691554435,-1.79976112765586,1.16693900049615));
#16101=CARTESIAN_POINT('Ctrl Pts',(3.60256173061535,-1.96669387239445,-0.861011438315259));
#16102=CARTESIAN_POINT('Ctrl Pts',(3.71262654568635,-0.359954108516095,
-2.11456895788097));
#16103=CARTESIAN_POINT('Ctrl Pts',(3.78600308906702,0.918995978500612,-1.68278800281661));
#16104=CARTESIAN_POINT('Ctrl Pts',(3.82269136075736,1.32903061802968,-1.24512073475524));
#16105=CARTESIAN_POINT('Ctrl Pts',(0.377308639242645,0.980771099081388,
-1.37424797458506));
#16106=CARTESIAN_POINT('Ctrl Pts',(0.413996910932979,1.4333290375638,-1.05126714802977));
#16107=CARTESIAN_POINT('Ctrl Pts',(0.487373454313646,1.98727149052022,0.0708647233282483));
#16108=CARTESIAN_POINT('Ctrl Pts',(0.597438269384649,1.03287962082695,1.70133053548414));
#16109=CARTESIAN_POINT('Ctrl Pts',(0.707503084455651,-0.851076859951723,
1.79718318835854));
#16110=CARTESIAN_POINT('Ctrl Pts',(0.817567899526653,-1.96933159241256,
0.279457815251136));
#16111=CARTESIAN_POINT('Ctrl Pts',(0.927632714597655,-1.31703478496902,
-1.49079722593874));
#16112=CARTESIAN_POINT('Ctrl Pts',(1.03769752966866,0.519628460241746,-1.91990990104726));
#16113=CARTESIAN_POINT('Ctrl Pts',(1.14776234473966,1.88899150129125,-0.623023827409443));
#16114=CARTESIAN_POINT('Ctrl Pts',(1.25782715981066,1.55984875606694,1.23424934804874));
#16115=CARTESIAN_POINT('Ctrl Pts',(1.36789197488167,-0.171891574044375,
1.9816202814377));
#16116=CARTESIAN_POINT('Ctrl Pts',(1.47795678995266,-1.74906201439294,0.947212036295147));
#16117=CARTESIAN_POINT('Ctrl Pts',(1.58802160502367,-1.75352024261074,-0.938933296255988));
#16118=CARTESIAN_POINT('Ctrl Pts',(1.69808642009467,-0.181250463897452,
-1.98079776834194));
#16119=CARTESIAN_POINT('Ctrl Pts',(1.80815123516567,1.55399438284826,-1.24158084366963));
#16120=CARTESIAN_POINT('Ctrl Pts',(1.91821605023667,1.8919233506961,0.614041041910564));
#16121=CARTESIAN_POINT('Ctrl Pts',(2.02828086530768,0.528677589947831,1.91752925636392));
#16122=CARTESIAN_POINT('Ctrl Pts',(2.13834568037868,-1.30994315312314,1.49681968436671));
#16123=CARTESIAN_POINT('Ctrl Pts',(2.24841049544968,-1.9706923156075,-0.269796664786988));
#16124=CARTESIAN_POINT('Ctrl Pts',(2.35847531052068,-0.859440654288179,
-1.79381775211878));
#16125=CARTESIAN_POINT('Ctrl Pts',(2.46854012559169,1.02460244851252,-1.70487869239822));
#16126=CARTESIAN_POINT('Ctrl Pts',(2.57860494066268,1.98734259132718,-0.0829515185421386));
#16127=CARTESIAN_POINT('Ctrl Pts',(2.68866975573369,1.16311648309291,1.6135640745943));
#16128=CARTESIAN_POINT('Ctrl Pts',(2.79873457080469,-0.706971119836928,
1.85919886177117));
#16129=CARTESIAN_POINT('Ctrl Pts',(2.9087993858757,-1.9413404231465,0.433085458645317));
#16130=CARTESIAN_POINT('Ctrl Pts',(3.01886420094669,-1.43015002979249,-1.38245089867482));
#16131=CARTESIAN_POINT('Ctrl Pts',(3.1289290160177,0.367093481335958,-1.95491430948549));
#16132=CARTESIAN_POINT('Ctrl Pts',(3.2389938310887,1.83407391379467,-0.769571727372066));
#16133=CARTESIAN_POINT('Ctrl Pts',(3.3490586461597,1.65224259315707,1.10776866133802));
#16134=CARTESIAN_POINT('Ctrl Pts',(3.4591234612307,-0.0159090843070601,
1.98899735857432));
#16135=CARTESIAN_POINT('Ctrl Pts',(3.56918827630171,-1.6684890842092,1.08182411229303));
#16136=CARTESIAN_POINT('Ctrl Pts',(3.6792530913727,-1.82324598950817,-0.798210475897646));
#16137=CARTESIAN_POINT('Ctrl Pts',(3.78931790644371,-0.333699562484492,
-1.96033527439683));
#16138=CARTESIAN_POINT('Ctrl Pts',(3.86269444982438,0.851965705336433,-1.5600478144534));
#16139=CARTESIAN_POINT('Ctrl Pts',(3.89938272151471,1.23209299539129,-1.15430338089783));
#16140=CARTESIAN_POINT('Ctrl Pts',(0.454,0.903606778650207,-1.26612599672284));
#16141=CARTESIAN_POINT('Ctrl Pts',(0.490688271690334,1.32055872730335,-0.9685563961068));
#16142=CARTESIAN_POINT('Ctrl Pts',(0.564064815071002,1.83091854106863,0.0652892855698468));
#16143=CARTESIAN_POINT('Ctrl Pts',(0.674129630142005,0.951615547993874,
1.56747461872394));
#16144=CARTESIAN_POINT('Ctrl Pts',(0.784194445213006,-0.784116518650487,
1.65578585359825));
#16145=CARTESIAN_POINT('Ctrl Pts',(0.894259260284009,-1.81439010384861,
0.257470857822195));
#16146=CARTESIAN_POINT('Ctrl Pts',(1.00432407535501,-1.21341418046553,-1.37350547973211));
#16147=CARTESIAN_POINT('Ctrl Pts',(1.11438889042601,0.478745549796269,-1.76885677260357));
#16148=CARTESIAN_POINT('Ctrl Pts',(1.22445370549702,1.74037094585896,-0.574006059349687));
#16149=CARTESIAN_POINT('Ctrl Pts',(1.33451852056802,1.4371242290595,1.13714206962872));
#16150=CARTESIAN_POINT('Ctrl Pts',(1.44458333563902,-0.158367626905839,
1.82571195327325));
#16151=CARTESIAN_POINT('Ctrl Pts',(1.55464815071002,-1.61145071868996,0.872688048839352));
#16152=CARTESIAN_POINT('Ctrl Pts',(1.66471296578102,-1.61555818601047,-0.865060656856582));
#16153=CARTESIAN_POINT('Ctrl Pts',(1.77477778085203,-0.166990185543427,
-1.82495415320191));
#16154=CARTESIAN_POINT('Ctrl Pts',(1.88484259592303,1.43173046151262,-1.14389674372839));
#16155=CARTESIAN_POINT('Ctrl Pts',(1.99490741099403,1.74307212557223,0.565730014230139));
#16156=CARTESIAN_POINT('Ctrl Pts',(2.10497222606503,0.487082719346801,1.76666343036964));
#16157=CARTESIAN_POINT('Ctrl Pts',(2.21503704113604,-1.20688049833151,1.37905410801525));
#16158=CARTESIAN_POINT('Ctrl Pts',(2.32510185620703,-1.81564376915743,-0.248569819591012));
#16159=CARTESIAN_POINT('Ctrl Pts',(2.43516667127804,-0.791822273096899,
-1.65268520044665));
#16160=CARTESIAN_POINT('Ctrl Pts',(2.54523148634904,0.943989600391651,-1.57074361659946));
#16161=CARTESIAN_POINT('Ctrl Pts',(2.65529630142005,1.83098404786343,-0.0764251256222896));
#16162=CARTESIAN_POINT('Ctrl Pts',(2.76536111649104,1.0716057390628,1.48661337691892));
#16163=CARTESIAN_POINT('Ctrl Pts',(2.87542593156205,-0.65134861415973,1.71292230769104));
#16164=CARTESIAN_POINT('Ctrl Pts',(2.98549074663305,-1.78860120130565,0.399011508937487));
#16165=CARTESIAN_POINT('Ctrl Pts',(3.09555556170405,-1.31762983495097,-1.27368353774256));
#16166=CARTESIAN_POINT('Ctrl Pts',(3.20562037677505,0.33821159539077,-1.80110713232262));
#16167=CARTESIAN_POINT('Ctrl Pts',(3.31568519184605,1.6897741201822,-0.709023981398171));
#16168=CARTESIAN_POINT('Ctrl Pts',(3.42575000691706,1.52224877807848,1.02061252875298));
#16169=CARTESIAN_POINT('Ctrl Pts',(3.53581482198805,-0.0146574021557552,
1.8325086226628));
#16170=CARTESIAN_POINT('Ctrl Pts',(3.64587963705906,-1.53721704076253,0.996709224089919));
#16171=CARTESIAN_POINT('Ctrl Pts',(3.75594445213006,-1.67979810662189,-0.735409513480033));
#16172=CARTESIAN_POINT('Ctrl Pts',(3.86600926720107,-0.307445016452888,
-1.8061015909127));
#16173=CARTESIAN_POINT('Ctrl Pts',(3.93938581058173,0.784935432172254,-1.43730762609018));
#16174=CARTESIAN_POINT('Ctrl Pts',(3.97607408227207,1.13515537275291,-1.06348602704042));
#16175=CARTESIAN_POINT('Ctrl Pts',(3.746,1.42596824066807,-1.33593808861265));
#16176=CARTESIAN_POINT('Ctrl Pts',(3.70931172830967,0.98602625166479,-1.80552819117983));
#16177=CARTESIAN_POINT('Ctrl Pts',(3.67262345661933,0.299908798558548,-2.03716541627246));
#16178=CARTESIAN_POINT('Ctrl Pts',(3.635935184929,-0.330472111450079,-1.92881898871341));
#16179=CARTESIAN_POINT('Ctrl Pts',(3.59924691323867,-0.96085302145871,-1.82047256115436));
#16180=CARTESIAN_POINT('Ctrl Pts',(3.56255864154833,-1.53549738836972,-1.37214248094361));
#16181=CARTESIAN_POINT('Ctrl Pts',(3.525870369858,-1.79296814112886,-0.785333059266217));
#16182=CARTESIAN_POINT('Ctrl Pts',(3.51053681061341,-1.90057590947793,-0.540080922329393));
#16183=CARTESIAN_POINT('Ctrl Pts',(3.49520325136882,-1.95278128848461,-0.270639867873916));
#16184=CARTESIAN_POINT('Ctrl Pts',(3.47986969212423,-1.95164700307266,-0.000819222043828699));
#16185=CARTESIAN_POINT('Origin',(4.,1.38777878078145E-16,1.15470053837925));
#16186=CARTESIAN_POINT('',(4.,7.07050159149938E-17,1.15470053837925));
#16187=CARTESIAN_POINT('',(4.,1.,0.577350269189626));
#16188=CARTESIAN_POINT('',(4.,0.25,1.01036297108185));
#16189=CARTESIAN_POINT('',(2.,1.38777878078145E-16,1.15470053837925));
#16190=CARTESIAN_POINT('',(4.,7.07050159149938E-17,1.15470053837925));
#16191=CARTESIAN_POINT('',(2.,1.,0.577350269189626));
#16192=CARTESIAN_POINT('',(2.,1.,0.577350269189626));
#16193=CARTESIAN_POINT('',(4.,1.,0.577350269189626));
#16194=CARTESIAN_POINT('Origin',(4.,-1.,0.577350269189626));
#16195=CARTESIAN_POINT('',(4.,-1.,0.577350269189626));
#16196=CARTESIAN_POINT('',(4.,-0.75,0.721687836487032));
#16197=CARTESIAN_POINT('',(2.,-1.,0.577350269189626));
#16198=CARTESIAN_POINT('',(4.,-1.,0.577350269189626));
#16199=CARTESIAN_POINT('',(2.,7.07050159149938E-17,1.15470053837925));
#16200=CARTESIAN_POINT('Origin',(4.,-1.,-0.577350269189626));
#16201=CARTESIAN_POINT('',(4.,-1.,-0.577350269189626));
#16202=CARTESIAN_POINT('',(4.,-1.,-0.288675134594813));
#16203=CARTESIAN_POINT('',(2.,-1.,-0.577350269189626));
#16204=CARTESIAN_POINT('',(4.,-1.,-0.577350269189626));
#16205=CARTESIAN_POINT('',(2.,-1.,0.577350269189626));
#16206=CARTESIAN_POINT('Origin',(4.,-2.77555756156289E-16,-1.15470053837925));
#16207=CARTESIAN_POINT('',(4.,-2.12115047744981E-16,-1.15470053837925));
#16208=CARTESIAN_POINT('',(4.,-0.25,-1.01036297108185));
#16209=CARTESIAN_POINT('',(2.,-2.77555756156289E-16,-1.15470053837925));
#16210=CARTESIAN_POINT('',(4.,-2.12115047744981E-16,-1.15470053837925));
#16211=CARTESIAN_POINT('',(2.,-1.,-0.577350269189626));
#16212=CARTESIAN_POINT('Origin',(4.,1.,-0.577350269189626));
#16213=CARTESIAN_POINT('',(4.,1.,-0.577350269189626));
#16214=CARTESIAN_POINT('',(4.,0.75,-0.721687836487033));
#16215=CARTESIAN_POINT('',(2.,1.,-0.577350269189626));
#16216=CARTESIAN_POINT('',(4.,1.,-0.577350269189626));
#16217=CARTESIAN_POINT('',(2.,-2.12115047744981E-16,-1.15470053837925));
#16218=CARTESIAN_POINT('Origin',(4.,1.,0.577350269189626));
#16219=CARTESIAN_POINT('',(4.,1.,0.288675134594813));
#16220=CARTESIAN_POINT('',(2.,1.,-0.577350269189626));
#16221=CARTESIAN_POINT('Origin',(2.,0.,0.));
#16222=CARTESIAN_POINT('Origin',(0.,1.5,0.));
#16223=CARTESIAN_POINT('',(1.04083408558608E-16,-1.5,-1.83697019872103E-16));
#16224=CARTESIAN_POINT('Origin',(0.,0.,0.));
#16225=CARTESIAN_POINT('Origin',(0.25,0.,0.));
#16226=CARTESIAN_POINT('',(0.25,-1.75,-2.14313189850787E-16));
#16227=CARTESIAN_POINT('Origin',(2.1,0.,0.));
#16228=CARTESIAN_POINT('Origin',(3.746,0.,0.));
#16229=CARTESIAN_POINT('Origin',(3.85,0.,0.));
#16230=CARTESIAN_POINT('',(4.,-1.7,-2.0818995585505E-16));
#16231=CARTESIAN_POINT('Origin',(4.,0.,0.));
#16232=CARTESIAN_POINT('',(3.85,-1.85,-2.2655965784226E-16));
#16233=CARTESIAN_POINT('Origin',(4.,0.,0.));
#16234=CARTESIAN_POINT('',(0.,0.,0.));
#16235=CARTESIAN_POINT('Origin',(-4.675,0.,0.));
#16236=CARTESIAN_POINT('',(-7.57584495415709,-1.46476825295553,0.00111815863164652));
#16237=CARTESIAN_POINT('',(-7.64715504584291,-1.46461339238561,0.00160511507277402));
#16238=CARTESIAN_POINT('',(-4.675,-1.4635,-1.79227059055215E-16));
#16239=CARTESIAN_POINT('',(-7.7365,0.63476680905654,1.31983838594169));
#16240=CARTESIAN_POINT('Ctrl Pts',(-7.57584495415709,-1.46476825295553,
0.00111815863164652));
#16241=CARTESIAN_POINT('Ctrl Pts',(-7.57949510849532,-1.46530187760278,
0.0680739723037402));
#16242=CARTESIAN_POINT('Ctrl Pts',(-7.58314526283355,-1.4611010846802,0.134958986929198));
#16243=CARTESIAN_POINT('Ctrl Pts',(-7.58679541717177,-1.45193482378899,
0.201151768713104));
#16244=CARTESIAN_POINT('Ctrl Pts',(-7.6130189523592,-1.38608233023814,0.676695699578037));
#16245=CARTESIAN_POINT('Ctrl Pts',(-7.63924248754663,-1.06394659683228,
1.11651134128917));
#16246=CARTESIAN_POINT('Ctrl Pts',(-7.66546602273406,-0.630444354550018,
1.32315907101614));
#16247=CARTESIAN_POINT('Ctrl Pts',(-7.68914401515605,-0.239022575056683,
1.50974731487885));
#16248=CARTESIAN_POINT('Ctrl Pts',(-7.71282200757803,0.243194194034392,
1.50623820939729));
#16249=CARTESIAN_POINT('Ctrl Pts',(-7.7365,0.635526523537879,1.32063649424652));
#16250=CARTESIAN_POINT('',(-7.7365,-0.634007094575234,1.31904027763684));
#16251=CARTESIAN_POINT('Origin',(-7.7365,0.,0.));
#16252=CARTESIAN_POINT('Ctrl Pts',(-7.7365,-0.634007094575232,1.31904027763684));
#16253=CARTESIAN_POINT('Ctrl Pts',(-7.71027646481257,-1.06867658660948,
1.11011296403058));
#16254=CARTESIAN_POINT('Ctrl Pts',(-7.68405292962514,-1.38849610006321,
0.67151411483421));
#16255=CARTESIAN_POINT('Ctrl Pts',(-7.65782939443771,-1.45248317015234,
0.196425540089081));
#16256=CARTESIAN_POINT('Ctrl Pts',(-7.65427127823944,-1.46116519677219,
0.13196358477567));
#16257=CARTESIAN_POINT('Ctrl Pts',(-7.65071316204118,-1.46513730485639,
0.0668298474456289));
#16258=CARTESIAN_POINT('Ctrl Pts',(-7.64715504584291,-1.46461339238561,
0.00160511507277402));
#16259=CARTESIAN_POINT('Origin',(-4.675,0.,0.));
#16260=CARTESIAN_POINT('',(-7.07584495415709,-1.46119452374026,4.09982538755738E-5));
#16261=CARTESIAN_POINT('',(-7.14715504584291,-1.46119347856455,7.51979904560513E-5));
#16262=CARTESIAN_POINT('',(-4.675,-1.4635,-1.79227059055215E-16));
#16263=CARTESIAN_POINT('Ctrl Pts',(-7.07584495415709,-1.46119452374026,
4.09982538755738E-5));
#16264=CARTESIAN_POINT('Ctrl Pts',(-7.0888205640374,-1.46125337597131,0.239559405180254));
#16265=CARTESIAN_POINT('Ctrl Pts',(-7.10179617391772,-1.40553952388032,
0.479051677557368));
#16266=CARTESIAN_POINT('Ctrl Pts',(-7.11477178379803,-1.29390043969062,
0.688772464510923));
#16267=CARTESIAN_POINT('Ctrl Pts',(-7.14099531898546,-1.06827933366594,
1.11261538880818));
#16268=CARTESIAN_POINT('Ctrl Pts',(-7.16721885417289,-0.614237919779222,
1.41486003607089));
#16269=CARTESIAN_POINT('Ctrl Pts',(-7.19344238936032,-0.136158112004879,
1.45946419653017));
#16270=CARTESIAN_POINT('Ctrl Pts',(-7.21966592454776,0.341921695769462,
1.50406835698944));
#16271=CARTESIAN_POINT('Ctrl Pts',(-7.24588945973518,0.844039897431429,
1.29103203064527));
#16272=CARTESIAN_POINT('Ctrl Pts',(-7.27211299492261,1.14416757992326,0.916230695246649));
#16273=CARTESIAN_POINT('Ctrl Pts',(-7.29833653011004,1.44429526241508,0.541429359848023));
#16274=CARTESIAN_POINT('Ctrl Pts',(-7.32456006529747,1.54243242573677,0.00486301539493375));
#16275=CARTESIAN_POINT('Ctrl Pts',(-7.3507836004849,1.39441016989669,-0.45189562140554));
#16276=CARTESIAN_POINT('Ctrl Pts',(-7.37700713567233,1.2463879140566,-0.908654258206013));
#16277=CARTESIAN_POINT('Ctrl Pts',(-7.40323067085976,0.85220623905475,-1.28560518735387));
#16278=CARTESIAN_POINT('Ctrl Pts',(-7.42945420604719,0.389290336756425,
-1.41314406620906));
#16279=CARTESIAN_POINT('Ctrl Pts',(-7.45567774123462,-0.0736255655419018,
-1.54068294506426));
#16280=CARTESIAN_POINT('Ctrl Pts',(-7.48190127642205,-0.605275695136702,
-1.41880977362678));
#16281=CARTESIAN_POINT('Ctrl Pts',(-7.50812481160948,-0.966316133086186,
-1.10223707789867));
#16282=CARTESIAN_POINT('Ctrl Pts',(-7.53069819245869,-1.27710196915086,
-0.829729348637408));
#16283=CARTESIAN_POINT('Ctrl Pts',(-7.55327157330789,-1.46146819732044,
-0.412951752401925));
#16284=CARTESIAN_POINT('Ctrl Pts',(-7.57584495415709,-1.46476825295553,
0.00111815863164652));
#16285=CARTESIAN_POINT('Ctrl Pts',(-7.64715504584291,-1.46461339238561,
0.00160511507277402));
#16286=CARTESIAN_POINT('Ctrl Pts',(-7.62448962685375,-1.46127603772873,
-0.413880441134546));
#16287=CARTESIAN_POINT('Ctrl Pts',(-7.60182420786459,-1.27550058420875,
-0.833058365384661));
#16288=CARTESIAN_POINT('Ctrl Pts',(-7.57915878887542,-0.962575882149317,
-1.10580548228527));
#16289=CARTESIAN_POINT('Ctrl Pts',(-7.55293525368799,-0.600526897332635,
-1.4213696296206));
#16290=CARTESIAN_POINT('Ctrl Pts',(-7.52671171850056,-0.0682743009747437,
-1.54091962399734));
#16291=CARTESIAN_POINT('Ctrl Pts',(-7.50048818331313,0.394239944793519,
-1.41166012590963));
#16292=CARTESIAN_POINT('Ctrl Pts',(-7.4742646481257,0.856754190561782,-1.28240062782193));
#16293=CARTESIAN_POINT('Ctrl Pts',(-7.44804111293827,1.24953008574042,-0.904331637269769));
#16294=CARTESIAN_POINT('Ctrl Pts',(-7.42181757775084,1.3959439261357,-0.447121059668684));
#16295=CARTESIAN_POINT('Ctrl Pts',(-7.39559404256341,1.54235776653098,0.0100895179324009));
#16296=CARTESIAN_POINT('Ctrl Pts',(-7.36937050737598,1.4424095521429,0.546441682582412));
#16297=CARTESIAN_POINT('Ctrl Pts',(-7.34314697218855,1.14099511095998,0.92023014033236));
#16298=CARTESIAN_POINT('Ctrl Pts',(-7.31692343700112,0.839580669777048,
1.29401859808231));
#16299=CARTESIAN_POINT('Ctrl Pts',(-7.29069990181369,0.336700001799267,
1.50524334893219));
#16300=CARTESIAN_POINT('Ctrl Pts',(-7.26447636662626,-0.141228388432861,
1.45896449548521));
#16301=CARTESIAN_POINT('Ctrl Pts',(-7.23825283143883,-0.619156778664989,
1.41268564203822));
#16302=CARTESIAN_POINT('Ctrl Pts',(-7.2120292962514,-1.07213289115146,1.10890318429437));
#16303=CARTESIAN_POINT('Ctrl Pts',(-7.18580576106397,-1.29627871914772,
0.684288464279752));
#16304=CARTESIAN_POINT('Ctrl Pts',(-7.17292218932362,-1.40640112768838,
0.47567607970926));
#16305=CARTESIAN_POINT('Ctrl Pts',(-7.16003861758326,-1.4612899065398,0.23789795580647));
#16306=CARTESIAN_POINT('Ctrl Pts',(-7.14715504584291,-1.46119347856455,
7.51979904560513E-5));
#16307=CARTESIAN_POINT('Origin',(-4.675,0.,0.));
#16308=CARTESIAN_POINT('',(-6.57584495415709,-1.46465303558881,-0.00106776041762152));
#16309=CARTESIAN_POINT('',(-6.64715504584291,-1.46460737782915,-0.00108331802881356));
#16310=CARTESIAN_POINT('',(-4.675,-1.4635,-1.79227059055215E-16));
#16311=CARTESIAN_POINT('Ctrl Pts',(-6.57584495415709,-1.46465303558881,
-0.00106776041762152));
#16312=CARTESIAN_POINT('Ctrl Pts',(-6.59814601957949,-1.46128671630142,
0.408115865061178));
#16313=CARTESIAN_POINT('Ctrl Pts',(-6.62044708500189,-1.28183534078177,
0.819889960702766));
#16314=CARTESIAN_POINT('Ctrl Pts',(-6.64274815042429,-0.977572876370026,
1.09221589872146));
#16315=CARTESIAN_POINT('Ctrl Pts',(-6.66897168561172,-0.619794568895003,
1.4124404567334));
#16316=CARTESIAN_POINT('Ctrl Pts',(-6.69519522079915,-0.089438661254516,
1.53984858630397));
#16317=CARTESIAN_POINT('Ctrl Pts',(-6.72141875598658,0.374758584894471,
1.41708857457618));
#16318=CARTESIAN_POINT('Ctrl Pts',(-6.74764229117401,0.838955831043458,
1.2943285628484));
#16319=CARTESIAN_POINT('Ctrl Pts',(-6.77386582636144,1.23699441570095,0.921400409822262));
#16320=CARTESIAN_POINT('Ctrl Pts',(-6.80008936154887,1.38969975267005,0.466174873903159));
#16321=CARTESIAN_POINT('Ctrl Pts',(-6.8263128967363,1.54240508963915,0.0109493379840572));
#16322=CARTESIAN_POINT('Ctrl Pts',(-6.85253643192373,1.44977717891987,-0.526573580828016));
#16323=CARTESIAN_POINT('Ctrl Pts',(-6.87875996711116,1.1535120245824,-0.904430536719963));
#16324=CARTESIAN_POINT('Ctrl Pts',(-6.90498350229859,0.857246870244925,
-1.28228749261191));
#16325=CARTESIAN_POINT('Ctrl Pts',(-6.93120703748602,0.357344472289264,
-1.50047848558374));
#16326=CARTESIAN_POINT('Ctrl Pts',(-6.95743057267345,-0.121167596084266,
-1.46078787938538));
#16327=CARTESIAN_POINT('Ctrl Pts',(-6.98365410786088,-0.599679664457794,
-1.42109727318701));
#16328=CARTESIAN_POINT('Ctrl Pts',(-7.00987764304832,-1.05680140324919,
-1.12352506781847));
#16329=CARTESIAN_POINT('Ctrl Pts',(-7.03610117823574,-1.28676187356357,
-0.702018364468302));
#16330=CARTESIAN_POINT('Ctrl Pts',(-7.04934910354286,-1.40293610836982,
-0.489076467713321));
#16331=CARTESIAN_POINT('Ctrl Pts',(-7.06259702884998,-1.46113443639422,
-0.244504113221373));
#16332=CARTESIAN_POINT('Ctrl Pts',(-7.07584495415709,-1.46119452374026,
4.09982538755738E-5));
#16333=CARTESIAN_POINT('Ctrl Pts',(-7.14715504584291,-1.46119347856455,
7.51979904560513E-5));
#16334=CARTESIAN_POINT('Ctrl Pts',(-7.13381508239583,-1.46109363469431,
-0.246172268169273));
#16335=CARTESIAN_POINT('Ctrl Pts',(-7.12047511894875,-1.40204395744491,
-0.492467586504148));
#16336=CARTESIAN_POINT('Ctrl Pts',(-7.10713515550167,-1.28432021657575,
-0.706483940746703));
#16337=CARTESIAN_POINT('Ctrl Pts',(-7.08091162031424,-1.05290034250147,
-1.12719464347314));
#16338=CARTESIAN_POINT('Ctrl Pts',(-7.05468808512682,-0.594745050846875,
-1.42316906664063));
#16339=CARTESIAN_POINT('Ctrl Pts',(-7.02846454993939,-0.11609725943412,
-1.4611967717883));
#16340=CARTESIAN_POINT('Ctrl Pts',(-7.00224101475196,0.362550531978637,
-1.49922447693597));
#16341=CARTESIAN_POINT('Ctrl Pts',(-6.97601747956452,0.861690823149552,
-1.27930546406382));
#16342=CARTESIAN_POINT('Ctrl Pts',(-6.94979394437709,1.15664263658477,-0.900424064368463));
#16343=CARTESIAN_POINT('Ctrl Pts',(-6.92357040918966,1.45159445001998,-0.521542664673106));
#16344=CARTESIAN_POINT('Ctrl Pts',(-6.89734687400224,1.5423577857195,0.0163011218454547));
#16345=CARTESIAN_POINT('Ctrl Pts',(-6.87112333881481,1.38807410635408,0.470994697121732));
#16346=CARTESIAN_POINT('Ctrl Pts',(-6.84489980362738,1.23379042698866,0.925688272398011));
#16347=CARTESIAN_POINT('Ctrl Pts',(-6.81867626843994,0.834459732558295,
1.297231636432));
#16348=CARTESIAN_POINT('Ctrl Pts',(-6.79245273325251,0.369839221643031,
1.41837991588424));
#16349=CARTESIAN_POINT('Ctrl Pts',(-6.76622919806508,-0.0947812892722306,
1.53952819533647));
#16350=CARTESIAN_POINT('Ctrl Pts',(-6.74000566287766,-0.624691616672391,
1.41028139020694));
#16351=CARTESIAN_POINT('Ctrl Pts',(-6.71378212769023,-0.981356587747756,
1.08881755089876));
#16352=CARTESIAN_POINT('Ctrl Pts',(-6.69157310040779,-1.28342044056879,
0.816565959857179));
#16353=CARTESIAN_POINT('Ctrl Pts',(-6.66936407312535,-1.46122233297314,
0.406444783164266));
#16354=CARTESIAN_POINT('Ctrl Pts',(-6.64715504584291,-1.46460737782915,
-0.00108331802881356));
#16355=CARTESIAN_POINT('Origin',(-4.675,0.,0.));
#16356=CARTESIAN_POINT('',(-6.0758449541571,-1.46387947857031,0.00124550601554009));
#16357=CARTESIAN_POINT('',(-6.14715504584291,-1.46392911471344,0.00123902392529235));
#16358=CARTESIAN_POINT('',(-4.675,-1.4635,-1.79227059055215E-16));
#16359=CARTESIAN_POINT('Ctrl Pts',(-6.0758449541571,-1.46387947857031,0.00124550601554009));
#16360=CARTESIAN_POINT('Ctrl Pts',(-6.08124793993415,-1.46476817976019,
0.100516198434922));
#16361=CARTESIAN_POINT('Ctrl Pts',(-6.08665092571121,-1.45551439595261,
0.199622273041832));
#16362=CARTESIAN_POINT('Ctrl Pts',(-6.09205391148826,-1.43550278566529,
0.296506294697566));
#16363=CARTESIAN_POINT('Ctrl Pts',(-6.11827744667569,-1.33837590283036,
0.766735470902046));
#16364=CARTESIAN_POINT('Ctrl Pts',(-6.14450098186312,-0.987829908906021,
1.18462036689892));
#16365=CARTESIAN_POINT('Ctrl Pts',(-6.17072451705055,-0.541660829647773,
1.36205278094015));
#16366=CARTESIAN_POINT('Ctrl Pts',(-6.19694805223798,-0.095491750389521,
1.53948519498138));
#16367=CARTESIAN_POINT('Ctrl Pts',(-6.22317158742541,0.446300414202636,
1.47646512706695));
#16368=CARTESIAN_POINT('Ctrl Pts',(-6.24939512261284,0.839831405567041,
1.20136066058004));
#16369=CARTESIAN_POINT('Ctrl Pts',(-6.27561865780027,1.23336239693144,0.926256194093134));
#16370=CARTESIAN_POINT('Ctrl Pts',(-6.3018421929877,1.47863221506809,0.439067329033746));
#16371=CARTESIAN_POINT('Ctrl Pts',(-6.32806572817513,1.46523422670663,-0.0409010089182408));
#16372=CARTESIAN_POINT('Ctrl Pts',(-6.35428926336256,1.45183623834517,-0.520869346870228));
#16373=CARTESIAN_POINT('Ctrl Pts',(-6.38051279854999,1.17977044348559,-0.993617157714814));
#16374=CARTESIAN_POINT('Ctrl Pts',(-6.40673633373742,0.77150551348923,-1.24634003584463));
#16375=CARTESIAN_POINT('Ctrl Pts',(-6.43295986892485,0.363240583492865,
-1.49906291397444));
#16376=CARTESIAN_POINT('Ctrl Pts',(-6.45918340411228,-0.181223481640291,
-1.53176085938949));
#16377=CARTESIAN_POINT('Ctrl Pts',(-6.48540693929971,-0.616799689488656,
-1.32971513666244));
#16378=CARTESIAN_POINT('Ctrl Pts',(-6.51163047448714,-1.05237589733702,
-1.1276694139354));
#16379=CARTESIAN_POINT('Ctrl Pts',(-6.53785400967457,-1.3790642479006,-0.690880023066263));
#16380=CARTESIAN_POINT('Ctrl Pts',(-6.564077544862,-1.4498080695276,-0.215964834405035));
#16381=CARTESIAN_POINT('Ctrl Pts',(-6.56800001462703,-1.46038980457634,
-0.14492786493607));
#16382=CARTESIAN_POINT('Ctrl Pts',(-6.57192248439206,-1.46524512773213,
-0.0730378824223954));
#16383=CARTESIAN_POINT('Ctrl Pts',(-6.57584495415709,-1.46465303558881,
-0.00106776041762152));
#16384=CARTESIAN_POINT('Ctrl Pts',(-6.64715504584291,-1.46460737782915,
-0.00108331802881356));
#16385=CARTESIAN_POINT('Ctrl Pts',(-6.64314053793791,-1.46521925916732,
-0.0747481734472876));
#16386=CARTESIAN_POINT('Ctrl Pts',(-6.63912603003292,-1.4601322017168,-0.148328302081877));
#16387=CARTESIAN_POINT('Ctrl Pts',(-6.63511152212793,-1.44904998055347,
-0.220994103));
#16388=CARTESIAN_POINT('Ctrl Pts',(-6.6088879869405,-1.37665878753324,-0.695661044103762));
#16389=CARTESIAN_POINT('Ctrl Pts',(-6.58266445175308,-1.04845678674222,
-1.13131405282446));
#16390=CARTESIAN_POINT('Ctrl Pts',(-6.55644091656565,-0.612182151683762,
-1.3318471614882));
#16391=CARTESIAN_POINT('Ctrl Pts',(-6.53021738137822,-0.175907516625305,
-1.53238027015193));
#16392=CARTESIAN_POINT('Ctrl Pts',(-6.50399384619078,0.368439752700586,
-1.4977934787587));
#16393=CARTESIAN_POINT('Ctrl Pts',(-6.47777031100335,0.775825313355198,
-1.24365558141487));
#16394=CARTESIAN_POINT('Ctrl Pts',(-6.45154677581592,1.18321087400981,-0.989517684071032));
#16395=CARTESIAN_POINT('Ctrl Pts',(-6.4253232406285,1.45363472599314,-0.515828680776595));
#16396=CARTESIAN_POINT('Ctrl Pts',(-6.39909970544107,1.46536726876187,-0.0358167504139053));
#16397=CARTESIAN_POINT('Ctrl Pts',(-6.37287617025364,1.4770998115306,0.444195179948787));
#16398=CARTESIAN_POINT('Ctrl Pts',(-6.3466526350662,1.23014104508472,0.930530037379732));
#16399=CARTESIAN_POINT('Ctrl Pts',(-6.32042909987877,0.835657892526212,
1.20426737561557));
#16400=CARTESIAN_POINT('Ctrl Pts',(-6.29420556469134,0.441174739967705,
1.47800471385141));
#16401=CARTESIAN_POINT('Ctrl Pts',(-6.26798202950391,-0.100832798703432,
1.53914453289215));
#16402=CARTESIAN_POINT('Ctrl Pts',(-6.24175849431648,-0.546383526501062,
1.36016510324213));
#16403=CARTESIAN_POINT('Ctrl Pts',(-6.21553495912905,-0.991934254298693,
1.18118567359212));
#16404=CARTESIAN_POINT('Ctrl Pts',(-6.18931142394163,-1.34102817122282,
0.762086995251349));
#16405=CARTESIAN_POINT('Ctrl Pts',(-6.1630878887542,-1.43652288894978,0.291523661031353));
#16406=CARTESIAN_POINT('Ctrl Pts',(-6.1577769411171,-1.45586305196907,0.19622235210727));
#16407=CARTESIAN_POINT('Ctrl Pts',(-6.15246599348001,-1.46480139245222,
0.098810128720388));
#16408=CARTESIAN_POINT('Ctrl Pts',(-6.14715504584291,-1.46392911471344,
0.00123902392529235));
#16409=CARTESIAN_POINT('Origin',(-4.675,0.,0.));
#16410=CARTESIAN_POINT('',(-5.57584495415709,-1.46133774784058,-0.000461094909492699));
#16411=CARTESIAN_POINT('',(-5.64715504584291,-1.46132187471162,-0.000435916869068641));
#16412=CARTESIAN_POINT('',(-4.675,-1.4635,-1.79227059055215E-16));
#16413=CARTESIAN_POINT('Ctrl Pts',(-5.57584495415709,-1.46133774784058,
-0.000461094909492699));
#16414=CARTESIAN_POINT('Ctrl Pts',(-5.59057339547623,-1.46055568691757,
0.271345601813848));
#16415=CARTESIAN_POINT('Ctrl Pts',(-5.60530183679537,-1.3877585012757,0.543541520393028));
#16416=CARTESIAN_POINT('Ctrl Pts',(-5.62003027811452,-1.24559580904415,
0.772706484360848));
#16417=CARTESIAN_POINT('Ctrl Pts',(-5.64625381330195,-0.992479523261131,
1.1807276297163));
#16418=CARTESIAN_POINT('Ctrl Pts',(-5.67247734848938,-0.519469702169433,
1.45233762200152));
#16419=CARTESIAN_POINT('Ctrl Pts',(-5.69870088367681,-0.0394886755002852,
1.46527296946528));
#16420=CARTESIAN_POINT('Ctrl Pts',(-5.72492441886424,0.440492351168856,
1.47820831692904));
#16421=CARTESIAN_POINT('Ctrl Pts',(-5.75114795405167,0.927444583415449,
1.23246901957134));
#16422=CARTESIAN_POINT('Ctrl Pts',(-5.7773714892391,1.2021696047976,0.838673042208838));
#16423=CARTESIAN_POINT('Ctrl Pts',(-5.80359502442652,1.47689462617977,0.444877064846331));
#16424=CARTESIAN_POINT('Ctrl Pts',(-5.82981855961395,1.53939243669748,-0.0969755925209766));
#16425=CARTESIAN_POINT('Ctrl Pts',(-5.85604209480139,1.36153004874535,-0.542973440251071));
#16426=CARTESIAN_POINT('Ctrl Pts',(-5.88226562998882,1.18366766079323,-0.988971287981157));
#16427=CARTESIAN_POINT('Ctrl Pts',(-5.90848916517625,0.765445074371262,
-1.33911432607403));
#16428=CARTESIAN_POINT('Ctrl Pts',(-5.93471270036368,0.295122497836863,
-1.4357879168145));
#16429=CARTESIAN_POINT('Ctrl Pts',(-5.96093623555111,-0.175200078697542,
-1.53246150755497));
#16430=CARTESIAN_POINT('Ctrl Pts',(-5.98715977073854,-0.697622645344382,
-1.37566565094302));
#16431=CARTESIAN_POINT('Ctrl Pts',(-6.01338330592597,-1.03698004279505,
-1.03598099443101));
#16432=CARTESIAN_POINT('Ctrl Pts',(-6.03420385533634,-1.30641768386431,
-0.766283521367007));
#16433=CARTESIAN_POINT('Ctrl Pts',(-6.05502440474672,-1.46045484489581,
-0.381296747805956));
#16434=CARTESIAN_POINT('Ctrl Pts',(-6.0758449541571,-1.46387947857031,0.00124550601554009));
#16435=CARTESIAN_POINT('Ctrl Pts',(-6.14715504584291,-1.46392911471344,
0.00123902392529235));
#16436=CARTESIAN_POINT('Ctrl Pts',(-6.12624245829258,-1.46049440101887,
-0.382960635125922));
#16437=CARTESIAN_POINT('Ctrl Pts',(-6.10532987074223,-1.3049461447426,-0.769623748906194));
#16438=CARTESIAN_POINT('Ctrl Pts',(-6.0844172831919,-1.03337916355809,-1.03957277506268));
#16439=CARTESIAN_POINT('Ctrl Pts',(-6.05819374800447,-0.692845201909629,
-1.37807788683748));
#16440=CARTESIAN_POINT('Ctrl Pts',(-6.03197021281705,-0.169881760082907,
-1.53306012028788));
#16441=CARTESIAN_POINT('Ctrl Pts',(-6.00574667762961,0.300102532701756,
-1.4347552146932));
#16442=CARTESIAN_POINT('Ctrl Pts',(-5.97952314244219,0.770086825486424,
-1.33645030909852));
#16443=CARTESIAN_POINT('Ctrl Pts',(-5.95329960725475,1.18709196922903,-0.984858264458742));
#16444=CARTESIAN_POINT('Ctrl Pts',(-5.92707607206732,1.36340577873993,-0.538245981610891));
#16445=CARTESIAN_POINT('Ctrl Pts',(-5.90085253687989,1.53971958825083,-0.091633698763043));
#16446=CARTESIAN_POINT('Ctrl Pts',(-5.87462900169247,1.47534206353002,0.449998822292882));
#16447=CARTESIAN_POINT('Ctrl Pts',(-5.84840546650504,1.19925233388025,0.842839185985495));
#16448=CARTESIAN_POINT('Ctrl Pts',(-5.8221819313176,0.923162604230478,1.23567954967811));
#16449=CARTESIAN_POINT('Ctrl Pts',(-5.79595839613017,0.435360669651733,
1.47972775600741));
#16450=CARTESIAN_POINT('Ctrl Pts',(-5.76973486094274,-0.0445725656008746,
1.46512707331867));
#16451=CARTESIAN_POINT('Ctrl Pts',(-5.74351132575531,-0.524505800853484,
1.45052639062993));
#16452=CARTESIAN_POINT('Ctrl Pts',(-5.71728779056788,-0.996570336779956,
1.17727681892315));
#16453=CARTESIAN_POINT('Ctrl Pts',(-5.69106425538045,-1.24826935756838,
0.768379896395325));
#16454=CARTESIAN_POINT('Ctrl Pts',(-5.67642785220127,-1.38875264182939,
0.540158179755382));
#16455=CARTESIAN_POINT('Ctrl Pts',(-5.66179144902209,-1.46058761064619,
0.269679569506198));
#16456=CARTESIAN_POINT('Ctrl Pts',(-5.64715504584291,-1.46132187471162,
-0.000435916869068641));
#16457=CARTESIAN_POINT('Origin',(-4.675,0.,0.));
#16458=CARTESIAN_POINT('',(-5.07584495415709,-1.46540112296262,-0.000672431366979809));
#16459=CARTESIAN_POINT('',(-5.14715504584291,-1.46536904737311,-0.000697413730935374));
#16460=CARTESIAN_POINT('',(-4.675,-1.4635,-1.79227059055215E-16));
#16461=CARTESIAN_POINT('Ctrl Pts',(-5.07584495415709,-1.46540112296262,
-0.000672431366979809));
#16462=CARTESIAN_POINT('Ctrl Pts',(-5.09989885101832,-1.46285813334839,
0.440080771362054));
#16463=CARTESIAN_POINT('Ctrl Pts',(-5.12395274787955,-1.25017446102815,
0.882964196354943));
#16464=CARTESIAN_POINT('Ctrl Pts',(-5.14800664474077,-0.903318012573032,
1.1543832979786));
#16465=CARTESIAN_POINT('Ctrl Pts',(-5.1742301799282,-0.525175446587734,
1.45028414111565));
#16466=CARTESIAN_POINT('Ctrl Pts',(-5.20045371511563,0.0124360176124621,
1.54239381648727));
#16467=CARTESIAN_POINT('Ctrl Pts',(-5.22667725030307,0.467514036020018,
1.38924974594796));
#16468=CARTESIAN_POINT('Ctrl Pts',(-5.25290078549049,0.92259205442756,1.23610567540865));
#16469=CARTESIAN_POINT('Ctrl Pts',(-5.27912432067793,1.29513662704247,0.837707858958433));
#16470=CARTESIAN_POINT('Ctrl Pts',(-5.30534785586535,1.41744920979827,0.373392512153981));
#16471=CARTESIAN_POINT('Ctrl Pts',(-5.33157139105279,1.53976179255407,-0.0909228346504821));
#16472=CARTESIAN_POINT('Ctrl Pts',(-5.35779492624021,1.41184238545076,-0.621155711809182));
#16473=CARTESIAN_POINT('Ctrl Pts',(-5.38401846142764,1.09127308713034,-0.978625198834701));
#16474=CARTESIAN_POINT('Ctrl Pts',(-5.41024199661507,0.770703788809914,
-1.33609468586022));
#16475=CARTESIAN_POINT('Ctrl Pts',(-5.43646553180251,0.257484599272379,
-1.52080078275256));
#16476=CARTESIAN_POINT('Ctrl Pts',(-5.46268906698994,-0.2173621630815,-1.44959922756557));
#16477=CARTESIAN_POINT('Ctrl Pts',(-5.48891260217737,-0.692208925435379,
-1.37839767237858));
#16478=CARTESIAN_POINT('Ctrl Pts',(-5.5151361373648,-1.1286832606056,-1.05128846511227));
#16479=CARTESIAN_POINT('Ctrl Pts',(-5.54135967255222,-1.33030905295355,
-0.61551771226628));
#16480=CARTESIAN_POINT('Ctrl Pts',(-5.55285476642051,-1.41869177453332,
-0.424497482796187));
#16481=CARTESIAN_POINT('Ctrl Pts',(-5.5643498602888,-1.46194812225331,-0.212597832610591));
#16482=CARTESIAN_POINT('Ctrl Pts',(-5.57584495415709,-1.46133774784058,
-0.000461094909492699));
#16483=CARTESIAN_POINT('Ctrl Pts',(-5.64715504584291,-1.46132187471162,
-0.000435916869068641));
#16484=CARTESIAN_POINT('Ctrl Pts',(-5.63556791383466,-1.46190316606789,
-0.214276965095653));
#16485=CARTESIAN_POINT('Ctrl Pts',(-5.62398078182641,-1.41792323597311,
-0.427890431283265));
#16486=CARTESIAN_POINT('Ctrl Pts',(-5.61239364981816,-1.32816529847952,
-0.620129820373049));
#16487=CARTESIAN_POINT('Ctrl Pts',(-5.58617011463073,-1.12502871295185,
-1.05519834126473));
#16488=CARTESIAN_POINT('Ctrl Pts',(-5.5599465794433,-0.687422036246132,
-1.38079110969925));
#16489=CARTESIAN_POINT('Ctrl Pts',(-5.53372304425587,-0.212331100229578,
-1.45034463428116));
#16490=CARTESIAN_POINT('Ctrl Pts',(-5.50749950906844,0.262759835786984,
-1.51989815886308));
#16491=CARTESIAN_POINT('Ctrl Pts',(-5.48127597388101,0.775335031114387,
-1.33341243959239));
#16492=CARTESIAN_POINT('Ctrl Pts',(-5.45505243869358,1.09466205718752,-0.974832824031823));
#16493=CARTESIAN_POINT('Ctrl Pts',(-5.42882890350615,1.41398908326066,-0.616253208471257));
#16494=CARTESIAN_POINT('Ctrl Pts',(-5.40260536831872,1.54006794007953,-0.0855796966208218));
#16495=CARTESIAN_POINT('Ctrl Pts',(-5.37638183313129,1.41614504088793,0.378308442182405));
#16496=CARTESIAN_POINT('Ctrl Pts',(-5.35015829794386,1.29222214169632,0.84219658098563));
#16497=CARTESIAN_POINT('Ctrl Pts',(-5.32393476275643,0.918297486494231,
1.23929934674164));
#16498=CARTESIAN_POINT('Ctrl Pts',(-5.297711227569,0.462690854646623,1.39086348262469));
#16499=CARTESIAN_POINT('Ctrl Pts',(-5.27148769238157,0.00708422279901214,
1.54242761850773));
#16500=CARTESIAN_POINT('Ctrl Pts',(-5.24526415719414,-0.530204385694121,
1.4484531245178));
#16501=CARTESIAN_POINT('Ctrl Pts',(-5.21904062200671,-0.907317958243424,
1.15124201491802));
#16502=CARTESIAN_POINT('Ctrl Pts',(-5.19507876328544,-1.25190697275698,
0.879664191115139));
#16503=CARTESIAN_POINT('Ctrl Pts',(-5.17111690456418,-1.46275843823164,
0.438394712888951));
#16504=CARTESIAN_POINT('Ctrl Pts',(-5.14715504584291,-1.46536904737311,
-0.000697413730935374));
#16505=CARTESIAN_POINT('Origin',(-4.675,0.,0.));
#16506=CARTESIAN_POINT('',(-4.57584495415709,-1.46294334847319,0.0012518377109378));
#16507=CARTESIAN_POINT('',(-4.64715504584291,-1.46299075660548,0.00125694264917424));
#16508=CARTESIAN_POINT('',(-4.675,-1.4635,-1.79227059055215E-16));
#16509=CARTESIAN_POINT('Ctrl Pts',(-4.57584495415709,-1.46294334847319,
0.0012518377109378));
#16510=CARTESIAN_POINT('Ctrl Pts',(-4.58300077137298,-1.4640569200179,0.132943452584338));
#16511=CARTESIAN_POINT('Ctrl Pts',(-4.59015658858886,-1.44770968903095,
0.26436354906558));
#16512=CARTESIAN_POINT('Ctrl Pts',(-4.59731240580474,-1.412790863166,0.390648444827308));
#16513=CARTESIAN_POINT('Ctrl Pts',(-4.62353594099217,-1.28482573617244,
0.853437852066254));
#16514=CARTESIAN_POINT('Ctrl Pts',(-4.6497594761796,-0.907450989065814,
1.24726342130028));
#16515=CARTESIAN_POINT('Ctrl Pts',(-4.67598301136703,-0.450539437904677,
1.39484710466189));
#16516=CARTESIAN_POINT('Ctrl Pts',(-4.70220654655446,0.00637211325646751,
1.5424307880235));
#16517=CARTESIAN_POINT('Ctrl Pts',(-4.72843008174189,0.542820468472122,
1.44377258551269));
#16518=CARTESIAN_POINT('Ctrl Pts',(-4.75465361692932,0.917326849766136,
1.14328285266129));
#16519=CARTESIAN_POINT('Ctrl Pts',(-4.78087715211675,1.29183323106015,0.8427931198099));
#16520=CARTESIAN_POINT('Ctrl Pts',(-4.80710068730418,1.50439763843252,0.340471856617928));
#16521=CARTESIAN_POINT('Ctrl Pts',(-4.83332422249161,1.45933557059906,-0.13756424999078));
#16522=CARTESIAN_POINT('Ctrl Pts',(-4.85954775767904,1.4142735027656,-0.61560035659948));
#16523=CARTESIAN_POINT('Ctrl Pts',(-4.88577129286647,1.1115849597263,-1.06935130662492));
#16524=CARTESIAN_POINT('Ctrl Pts',(-4.9119948280539,0.687523242977742,-1.29456402732985));
#16525=CARTESIAN_POINT('Ctrl Pts',(-4.93821836324133,0.263461526229175,
-1.51977674803479));
#16526=CARTESIAN_POINT('Ctrl Pts',(-4.96444189842876,-0.281973364228664,
-1.51645123941922));
#16527=CARTESIAN_POINT('Ctrl Pts',(-4.99066543361619,-0.703257419359688,
-1.28608445780473));
#16528=CARTESIAN_POINT('Ctrl Pts',(-5.01688896880362,-1.12454147449071,
-1.05571767619023));
#16529=CARTESIAN_POINT('Ctrl Pts',(-5.04311250399105,-1.42167469429492,
-0.598309621576813));
#16530=CARTESIAN_POINT('Ctrl Pts',(-5.06933603917848,-1.46090447031182,
-0.119759588818864));
#16531=CARTESIAN_POINT('Ctrl Pts',(-5.07150567750469,-1.46415019690689,
-0.0801661287969205));
#16532=CARTESIAN_POINT('Ctrl Pts',(-5.07367531583089,-1.46563049817621,
-0.0404279456836342));
#16533=CARTESIAN_POINT('Ctrl Pts',(-5.07584495415709,-1.46540112296262,
-0.000672431366979809));
#16534=CARTESIAN_POINT('Ctrl Pts',(-5.14715504584291,-1.46536904737311,
-0.000697413730935374));
#16535=CARTESIAN_POINT('Ctrl Pts',(-5.14489336937675,-1.465615453686,-0.0421417916819987));
#16536=CARTESIAN_POINT('Ctrl Pts',(-5.14263169291058,-1.46400668068721,
-0.0835667720099182));
#16537=CARTESIAN_POINT('Ctrl Pts',(-5.14037001644442,-1.46048008062653,
-0.12482783486786));
#16538=CARTESIAN_POINT('Ctrl Pts',(-5.11414648125699,-1.41959009385488,
-0.603238849844358));
#16539=CARTESIAN_POINT('Ctrl Pts',(-5.08792294606956,-1.12087158370608,
-1.05961315458773));
#16540=CARTESIAN_POINT('Ctrl Pts',(-5.06169941088213,-0.698790766895836,
-1.28851679009923));
#16541=CARTESIAN_POINT('Ctrl Pts',(-5.0354758756947,-0.276709950085593,
-1.51742042561072));
#16542=CARTESIAN_POINT('Ctrl Pts',(-5.00925234050727,0.268733173386092,
-1.51885339189034));
#16543=CARTESIAN_POINT('Ctrl Pts',(-4.98302880531984,0.692010888444511,
-1.29217064838177));
#16544=CARTESIAN_POINT('Ctrl Pts',(-4.95680527013241,1.11528860350292,-1.0654879048732));
#16545=CARTESIAN_POINT('Ctrl Pts',(-4.93058173494498,1.41640091014807,-0.610689451576441));
#16546=CARTESIAN_POINT('Ctrl Pts',(-4.90435819975755,1.45980403956193,-0.132499888090858));
#16547=CARTESIAN_POINT('Ctrl Pts',(-4.87813466457012,1.50320716897579,0.345689675394735));
#16548=CARTESIAN_POINT('Ctrl Pts',(-4.85191112938269,1.28890112115835,0.847270349069159));
#16549=CARTESIAN_POINT('Ctrl Pts',(-4.82568759419526,0.913354385642052,
1.146458817618));
#16550=CARTESIAN_POINT('Ctrl Pts',(-4.79946405900783,0.537807650125757,
1.44564728616683));
#16551=CARTESIAN_POINT('Ctrl Pts',(-4.7732405238204,0.00102022691060563,
1.54244354959008));
#16552=CARTESIAN_POINT('Ctrl Pts',(-4.74701698863297,-0.455376476747224,
1.39327539226482));
#16553=CARTESIAN_POINT('Ctrl Pts',(-4.72079345344554,-0.911773180405061,
1.24410723493957));
#16554=CARTESIAN_POINT('Ctrl Pts',(-4.69456991825811,-1.28777916450557,
0.848974656865799));
#16555=CARTESIAN_POINT('Ctrl Pts',(-4.66834638307068,-1.41413775285701,
0.385744047536753));
#16556=CARTESIAN_POINT('Ctrl Pts',(-4.66128260399475,-1.4481747027221,0.260964582749956));
#16557=CARTESIAN_POINT('Ctrl Pts',(-4.65421882491883,-1.46409746841424,
0.131243987789252));
#16558=CARTESIAN_POINT('Ctrl Pts',(-4.64715504584291,-1.46299075660548,
0.00125694264917424));
#16559=CARTESIAN_POINT('Origin',(-4.675,0.,0.));
#16560=CARTESIAN_POINT('',(-4.0758449541571,-1.46180176082141,-0.000890585205371164));
#16561=CARTESIAN_POINT('',(-4.14715504584291,-1.46177010110622,-0.000870981035757715));
#16562=CARTESIAN_POINT('',(-4.675,-1.4635,-1.79227059055215E-16));
#16563=CARTESIAN_POINT('Ctrl Pts',(-4.0758449541571,-1.46180176082141,-0.000890585205371164));
#16564=CARTESIAN_POINT('Ctrl Pts',(-4.09232622691506,-1.46007789690811,
0.303021445376408));
#16565=CARTESIAN_POINT('Ctrl Pts',(-4.10880749967303,-1.36752126553833,
0.607895648754888));
#16566=CARTESIAN_POINT('Ctrl Pts',(-4.125288772431,-1.19185385646752,0.853269368559352));
#16567=CARTESIAN_POINT('Ctrl Pts',(-4.15151230761843,-0.912347500938886,
1.24368620528404));
#16568=CARTESIAN_POINT('Ctrl Pts',(-4.17773584280586,-0.422435044033784,
1.48346957273887));
#16569=CARTESIAN_POINT('Ctrl Pts',(-4.20395937799329,0.0573525716842393,
1.46468252976897));
#16570=CARTESIAN_POINT('Ctrl Pts',(-4.23018291318072,0.537140187402255,
1.44589548679908));
#16571=CARTESIAN_POINT('Ctrl Pts',(-4.25640644836815,1.00680296193319,1.16853803340446));
#16572=CARTESIAN_POINT('Ctrl Pts',(-4.28262998355558,1.25492521704804,0.757460843943328));
#16573=CARTESIAN_POINT('Ctrl Pts',(-4.30885351874301,1.50304747216288,0.346383654482191));
#16574=CARTESIAN_POINT('Ctrl Pts',(-4.33507705393044,1.52962920786163,-0.198413271045462));
#16575=CARTESIAN_POINT('Ctrl Pts',(-4.36130058911787,1.32270482672636,-0.631693099413778));
#16576=CARTESIAN_POINT('Ctrl Pts',(-4.3875241243053,1.11578044559109,-1.0649729277821));
#16577=CARTESIAN_POINT('Ctrl Pts',(-4.41374765949273,0.675349947621797,
-1.38673565899107));
#16578=CARTESIAN_POINT('Ctrl Pts',(-4.43997119468016,0.199670289708311,
-1.45214186837879));
#16579=CARTESIAN_POINT('Ctrl Pts',(-4.46619472986759,-0.276009368205169,
-1.5175480777665));
#16580=CARTESIAN_POINT('Ctrl Pts',(-4.49241826505502,-0.786938186062845,
-1.32659776533294));
#16581=CARTESIAN_POINT('Ctrl Pts',(-4.51864180024245,-1.10312484155144,
-0.965245986494234));
#16582=CARTESIAN_POINT('Ctrl Pts',(-4.537709518214,-1.33303121878594,-0.702499039594554));
#16583=CARTESIAN_POINT('Ctrl Pts',(-4.55677723618554,-1.45997607478309,
-0.349659664898473));
#16584=CARTESIAN_POINT('Ctrl Pts',(-4.57584495415709,-1.46294334847319,
0.0012518377109378));
#16585=CARTESIAN_POINT('Ctrl Pts',(-4.64715504584291,-1.46299075660548,
0.00125694264917424));
#16586=CARTESIAN_POINT('Ctrl Pts',(-4.6279952897314,-1.45998891748883,-0.351319214641563));
#16587=CARTESIAN_POINT('Ctrl Pts',(-4.6088355336199,-1.33169977541796,-0.705855668385529));
#16588=CARTESIAN_POINT('Ctrl Pts',(-4.58967577750839,-1.09976899462203,
-0.969067702863716));
#16589=CARTESIAN_POINT('Ctrl Pts',(-4.56345224232096,-0.782330455433243,
-1.32932020335082));
#16590=CARTESIAN_POINT('Ctrl Pts',(-4.53722870713353,-0.27074218445331,
-1.51849656374072));
#16591=CARTESIAN_POINT('Ctrl Pts',(-4.5110051719461,0.204707647421047,-1.45144026172377));
#16592=CARTESIAN_POINT('Ctrl Pts',(-4.48478163675867,0.680157479295415,
-1.38438395970681));
#16593=CARTESIAN_POINT('Ctrl Pts',(-4.45855810157124,1.11946887206421,-1.06109499528299));
#16594=CARTESIAN_POINT('Ctrl Pts',(-4.43233456638381,1.32488862684911,-0.627099817183438));
#16595=CARTESIAN_POINT('Ctrl Pts',(-4.40611103119638,1.53030838163401,-0.193104639083896));
#16596=CARTESIAN_POINT('Ctrl Pts',(-4.37988749600895,1.50183649843503,0.351596752691371));
#16597=CARTESIAN_POINT('Ctrl Pts',(-4.35366396082152,1.25228941241289,0.761810528821953));
#16598=CARTESIAN_POINT('Ctrl Pts',(-4.32744042563408,1.00274232639075,1.17202430495254));
#16599=CARTESIAN_POINT('Ctrl Pts',(-4.30121689044665,0.532120037545447,
1.44775046543844));
#16600=CARTESIAN_POINT('Ctrl Pts',(-4.27499335525922,0.0522701433084407,
1.46487265193383));
#16601=CARTESIAN_POINT('Ctrl Pts',(-4.24876982007179,-0.427579750928559,
1.48199483842921));
#16602=CARTESIAN_POINT('Ctrl Pts',(-4.22254628488437,-0.916657250557259,
1.24051305093409));
#16603=CARTESIAN_POINT('Ctrl Pts',(-4.19632274969694,-1.19480726366955,
0.849128763468167));
#16604=CARTESIAN_POINT('Ctrl Pts',(-4.17993351507893,-1.36864598492955,
0.60452067126266));
#16605=CARTESIAN_POINT('Ctrl Pts',(-4.16354428046092,-1.46009593122817,
0.301360308131175));
#16606=CARTESIAN_POINT('Ctrl Pts',(-4.14715504584291,-1.46177010110622,
-0.000870981035757715));
#16607=CARTESIAN_POINT('Origin',(-4.675,0.,0.));
#16608=CARTESIAN_POINT('',(-3.57584495415709,-1.46578812638883,-0.00013691639962482));
#16609=CARTESIAN_POINT('',(-3.64715504584291,-1.46577995658709,-0.000166956455778383));
#16610=CARTESIAN_POINT('',(-4.675,-1.4635,-1.79227059055215E-16));
#16611=CARTESIAN_POINT('Ctrl Pts',(-3.57584495415709,-1.46578812638883,
-0.00013691639962482));
#16612=CARTESIAN_POINT('Ctrl Pts',(-3.60165168245715,-1.46514662501551,
0.472401287906723));
#16613=CARTESIAN_POINT('Ctrl Pts',(-3.6274584107572,-1.21566859845595,0.945522380027992));
#16614=CARTESIAN_POINT('Ctrl Pts',(-3.65326513905726,-0.825120157214755,
1.21151184763414));
#16615=CARTESIAN_POINT('Ctrl Pts',(-3.67948867424469,-0.428263931496958,
1.48179733606006));
#16616=CARTESIAN_POINT('Ctrl Pts',(-3.70571220943212,0.114256391201713,
1.53820636350536));
#16617=CARTESIAN_POINT('Ctrl Pts',(-3.73193574461955,0.558228775463752,
1.35534676916974));
#16618=CARTESIAN_POINT('Ctrl Pts',(-3.75815927980698,1.00220115972579,1.17248717483412));
#16619=CARTESIAN_POINT('Ctrl Pts',(-3.78438281499441,1.3476256055512,0.750358958717571));
#16620=CARTESIAN_POINT('Ctrl Pts',(-3.81060635018184,1.43901151974464,0.27898042309323));
#16621=CARTESIAN_POINT('Ctrl Pts',(-3.83682988536927,1.53039743393808,-0.192398112531104));
#16622=CARTESIAN_POINT('Ctrl Pts',(-3.8630534205567,1.36774481649956,-0.713026967663235));
#16623=CARTESIAN_POINT('Ctrl Pts',(-3.88927695574413,1.02427069729705,-1.04854841051664));
#16624=CARTESIAN_POINT('Ctrl Pts',(-3.91550049093156,0.680796578094537,
-1.38406985337005));
#16625=CARTESIAN_POINT('Ctrl Pts',(-3.94172402611899,0.156500957128029,
-1.53448388394474));
#16626=CARTESIAN_POINT('Ctrl Pts',(-3.96794756130642,-0.312607862765557,
-1.43208259350458));
#16627=CARTESIAN_POINT('Ctrl Pts',(-3.99417109649385,-0.781716682659144,
-1.32968130306442));
#16628=CARTESIAN_POINT('Ctrl Pts',(-4.02039463168128,-1.19563870147981,
-0.974464691609415));
#16629=CARTESIAN_POINT('Ctrl Pts',(-4.04661816686871,-1.36804958381406,
-0.52633123288464));
#16630=CARTESIAN_POINT('Ctrl Pts',(-4.05636042929817,-1.43210166715789,
-0.359845908647675));
#16631=CARTESIAN_POINT('Ctrl Pts',(-4.06610269172764,-1.4628207558276,-0.180536344418141));
#16632=CARTESIAN_POINT('Ctrl Pts',(-4.0758449541571,-1.46180176082141,-0.000890585205371164));
#16633=CARTESIAN_POINT('Ctrl Pts',(-4.14715504584291,-1.46177010110622,
-0.000870981035757715));
#16634=CARTESIAN_POINT('Ctrl Pts',(-4.13732074527349,-1.46277468064693,
-0.182223765862292));
#16635=CARTESIAN_POINT('Ctrl Pts',(-4.12748644470407,-1.43145498611871,
-0.363242032373778));
#16636=CARTESIAN_POINT('Ctrl Pts',(-4.11765214413464,-1.36621505532258,
-0.53107483170888));
#16637=CARTESIAN_POINT('Ctrl Pts',(-4.09142860894721,-1.19225030726744,
-0.978607351983263));
#16638=CARTESIAN_POINT('Ctrl Pts',(-4.06520507375979,-0.777098284561283,
-1.33238560509529));
#16639=CARTESIAN_POINT('Ctrl Pts',(-4.03898153857236,-0.307637000979528,
-1.43315858504627));
#16640=CARTESIAN_POINT('Ctrl Pts',(-4.01275800338493,0.16182428260222,-1.53393156499725));
#16641=CARTESIAN_POINT('Ctrl Pts',(-3.98653446819749,0.685594827059569,
-1.38169927178719));
#16642=CARTESIAN_POINT('Ctrl Pts',(-3.96031093301006,1.02790268941062,-1.04498809341299));
#16643=CARTESIAN_POINT('Ctrl Pts',(-3.93408739782263,1.37021055176168,-0.708276915038779));
#16644=CARTESIAN_POINT('Ctrl Pts',(-3.9078638626352,1.53105573200644,-0.187086851500426));
#16645=CARTESIAN_POINT('Ctrl Pts',(-3.88164032744778,1.43803480643175,0.283971741109459));
#16646=CARTESIAN_POINT('Ctrl Pts',(-3.85541679226035,1.34501388085707,0.755030333719338));
#16647=CARTESIAN_POINT('Ctrl Pts',(-3.82919325707291,0.998126849462947,
1.17595745540075));
#16648=CARTESIAN_POINT('Ctrl Pts',(-3.80296972188548,0.55352267908109,1.35727546872357));
#16649=CARTESIAN_POINT('Ctrl Pts',(-3.77674618669805,0.108918508699223,
1.53859348204638));
#16650=CARTESIAN_POINT('Ctrl Pts',(-3.75052265151062,-0.433402800670376,
1.4803023870106));
#16651=CARTESIAN_POINT('Ctrl Pts',(-3.72429911632319,-0.829318798459288,
1.20864154522129));
#16652=CARTESIAN_POINT('Ctrl Pts',(-3.6985844261631,-1.21755238862171,0.942252047187829));
#16653=CARTESIAN_POINT('Ctrl Pts',(-3.672869736003,-1.46500727958381,0.470692975234204));
#16654=CARTESIAN_POINT('Ctrl Pts',(-3.64715504584291,-1.46577995658709,
-0.000166956455778383));
#16655=CARTESIAN_POINT('Origin',(-4.675,0.,0.));
#16656=CARTESIAN_POINT('',(-3.07584495415709,-1.46212013789102,0.00104925812874614));
#16657=CARTESIAN_POINT('',(-3.14715504584291,-1.46215854801559,0.001064531573891));
#16658=CARTESIAN_POINT('',(-4.675,-1.4635,-1.79227059055215E-16));
#16659=CARTESIAN_POINT('Ctrl Pts',(-3.07584495415709,-1.46212013789102,
0.00104925812874614));
#16660=CARTESIAN_POINT('Ctrl Pts',(-3.0847536028118,-1.46323398523221,0.165233158946807));
#16661=CARTESIAN_POINT('Ctrl Pts',(-3.09366225146651,-1.43767095884633,
0.329080475627605));
#16662=CARTESIAN_POINT('Ctrl Pts',(-3.10257090012123,-1.38391209651775,
0.483085407287739));
#16663=CARTESIAN_POINT('Ctrl Pts',(-3.12879443530866,-1.22566728604764,
0.936414963874487));
#16664=CARTESIAN_POINT('Ctrl Pts',(-3.15501797049609,-0.823111043591577,
1.30446216942745));
#16665=CARTESIAN_POINT('Ctrl Pts',(-3.18124150568352,-0.357451444629033,
1.42155292093755));
#16666=CARTESIAN_POINT('Ctrl Pts',(-3.20746504087095,0.108208154333504,
1.53864367244765));
#16667=CARTESIAN_POINT('Ctrl Pts',(-3.23368857605837,0.636971109802517,
1.40477796991489));
#16668=CARTESIAN_POINT('Ctrl Pts',(-3.2599121112458,0.990818161946596,1.08021460904761));
#16669=CARTESIAN_POINT('Ctrl Pts',(-3.28613564643324,1.34466521409068,0.755651248180315));
#16670=CARTESIAN_POINT('Ctrl Pts',(-3.31235918162067,1.52359636290982,0.240390228978487));
#16671=CARTESIAN_POINT('Ctrl Pts',(-3.3385827168081,1.44706691016575,-0.233627019133847));
#16672=CARTESIAN_POINT('Ctrl Pts',(-3.36480625199553,1.37053745742168,-0.707644267246182));
#16673=CARTESIAN_POINT('Ctrl Pts',(-3.39102978718296,1.03854740311439,-1.14041774426902));
#16674=CARTESIAN_POINT('Ctrl Pts',(-3.41725332237039,0.600539931461536,
-1.33713724918636));
#16675=CARTESIAN_POINT('Ctrl Pts',(-3.44347685755782,0.162532459808684,
-1.5338567541037));
#16676=CARTESIAN_POINT('Ctrl Pts',(-3.46970039274525,-0.381492429189738,
-1.49452228691555));
#16677=CARTESIAN_POINT('Ctrl Pts',(-3.49592392793268,-0.786645427391987,
-1.23684000663439));
#16678=CARTESIAN_POINT('Ctrl Pts',(-3.52214746312011,-1.19179842559424,
-0.97915772635323));
#16679=CARTESIAN_POINT('Ctrl Pts',(-3.54837099830754,-1.45807953300032,
-0.503127632979056));
#16680=CARTESIAN_POINT('Ctrl Pts',(-3.57459453349497,-1.46562402233489,
-0.0230316115886923));
#16681=CARTESIAN_POINT('Ctrl Pts',(-3.57501134038234,-1.46574393733086,
-0.0154007819966268));
#16682=CARTESIAN_POINT('Ctrl Pts',(-3.57542814726972,-1.46579848733764,
-0.00776892522355069));
#16683=CARTESIAN_POINT('Ctrl Pts',(-3.57584495415709,-1.46578812638883,
-0.00013691639962482));
#16684=CARTESIAN_POINT('Ctrl Pts',(-3.64715504584291,-1.46577995658709,
-0.000166956455778383));
#16685=CARTESIAN_POINT('Ctrl Pts',(-3.64664620081557,-1.46579524640192,
-0.00948438292758694));
#16686=CARTESIAN_POINT('Ctrl Pts',(-3.64613735578824,-1.46571394306979,
-0.0188015356376304));
#16687=CARTESIAN_POINT('Ctrl Pts',(-3.6456285107609,-1.4655352260066,-0.0281168194302507));
#16688=CARTESIAN_POINT('Ctrl Pts',(-3.61940497557347,-1.45632496955679,
-0.508183753749672));
#16689=CARTESIAN_POINT('Ctrl Pts',(-3.59318144038604,-1.18839377044896,
-0.983287033845705));
#16690=CARTESIAN_POINT('Ctrl Pts',(-3.56695790519861,-0.782349135137309,
-1.23956197302861));
#16691=CARTESIAN_POINT('Ctrl Pts',(-3.54073437001118,-0.376304499825653,
-1.49583691221152));
#16692=CARTESIAN_POINT('Ctrl Pts',(-3.51451083482375,0.167853571689824,
-1.53328351048129));
#16693=CARTESIAN_POINT('Ctrl Pts',(-3.48828729963632,0.60517582193308,-1.33504542211986));
#16694=CARTESIAN_POINT('Ctrl Pts',(-3.46206376444889,1.04249807217633,-1.13680733375844));
#16695=CARTESIAN_POINT('Ctrl Pts',(-3.43584022926146,1.37298450114736,-0.702884558765829));
#16696=CARTESIAN_POINT('Ctrl Pts',(-3.40961669407403,1.44786876825344,-0.228604644891952));
#16697=CARTESIAN_POINT('Ctrl Pts',(-3.3833931588866,1.52275303535953,0.245675268981927));
#16698=CARTESIAN_POINT('Ctrl Pts',(-3.35716962369917,1.34203514060067,0.760312321737079));
#16699=CARTESIAN_POINT('Ctrl Pts',(-3.33094608851174,0.987064081362439,
1.08364595394706));
#16700=CARTESIAN_POINT('Ctrl Pts',(-3.30472255332431,0.632093022124202,
1.40697958615704));
#16701=CARTESIAN_POINT('Ctrl Pts',(-3.27849901813688,0.102868798406588,
1.53900979782185));
#16702=CARTESIAN_POINT('Ctrl Pts',(-3.25227548294945,-0.362381706248886,
1.42030403618362));
#16703=CARTESIAN_POINT('Ctrl Pts',(-3.22605194776202,-0.827632210904352,
1.30159827454539));
#16704=CARTESIAN_POINT('Ctrl Pts',(-3.19982841257459,-1.22890899649768,
0.932156539604121));
#16705=CARTESIAN_POINT('Ctrl Pts',(-3.17360487738716,-1.38557990166134,
0.478280656560232));
#16706=CARTESIAN_POINT('Ctrl Pts',(-3.16478826687241,-1.43825420129137,
0.325683119491518));
#16707=CARTESIAN_POINT('Ctrl Pts',(-3.15597165635766,-1.46327897253593,
0.163541394970867));
#16708=CARTESIAN_POINT('Ctrl Pts',(-3.14715504584291,-1.46215854801559,
0.001064531573891));
#16709=CARTESIAN_POINT('Origin',(-4.675,0.,0.));
#16710=CARTESIAN_POINT('',(-2.57584495415709,-1.46253100424383,-0.00117902711067597));
#16711=CARTESIAN_POINT('',(-2.64715504584291,-1.46248673610352,-0.00116876785021116));
#16712=CARTESIAN_POINT('',(-4.675,-1.4635,-1.79227059055215E-16));
#16713=CARTESIAN_POINT('Ctrl Pts',(-2.57584495415709,-1.46253100424383,
-0.00117902711067597));
#16714=CARTESIAN_POINT('Ctrl Pts',(-2.59407905835389,-1.45991564447785,
0.334631950775567));
#16715=CARTESIAN_POINT('Ctrl Pts',(-2.61231316255069,-1.34476101557545,
0.672063525348569));
#16716=CARTESIAN_POINT('Ctrl Pts',(-2.63054726674748,-1.1329090593835,0.930107455118416));
#16717=CARTESIAN_POINT('Ctrl Pts',(-2.65677080193491,-0.828232330120255,
1.30121557203982));
#16718=CARTESIAN_POINT('Ctrl Pts',(-2.68299433712235,-0.323556481759576,
1.50812619278528));
#16719=CARTESIAN_POINT('Ctrl Pts',(-2.70921787230977,0.153943264898992,
1.45769889133524));
#16720=CARTESIAN_POINT('Ctrl Pts',(-2.7354414074972,0.63144301155756,1.40727158988519));
#16721=CARTESIAN_POINT('Ctrl Pts',(-2.76166494268463,1.08176665651402,1.09950636623965));
#16722=CARTESIAN_POINT('Ctrl Pts',(-2.78788847787206,1.30220318772352,0.672942251246367));
#16723=CARTESIAN_POINT('Ctrl Pts',(-2.81411201305949,1.52263971893302,0.246378136253079));
#16724=CARTESIAN_POINT('Ctrl Pts',(-2.84033554824692,1.51318913639555,-0.298984870087951));
#16725=CARTESIAN_POINT('Ctrl Pts',(-2.86655908343435,1.27810593674146,-0.717655376634697));
#16726=CARTESIAN_POINT('Ctrl Pts',(-2.89278261862179,1.04302273708737,-1.13632588318144));
#16727=CARTESIAN_POINT('Ctrl Pts',(-2.91900615380921,0.582306920316665,
-1.4283038899339));
#16728=CARTESIAN_POINT('Ctrl Pts',(-2.94522968899664,0.103346550680954,
-1.46215723795242));
#16729=CARTESIAN_POINT('Ctrl Pts',(-2.97145322418407,-0.375613818954749,
-1.49601058597093));
#16730=CARTESIAN_POINT('Ctrl Pts',(-2.9976767593715,-0.872818741455455,
-1.2717392752555));
#16731=CARTESIAN_POINT('Ctrl Pts',(-3.02390029455893,-1.16445451346373,
-0.890297666087522));
#16732=CARTESIAN_POINT('Ctrl Pts',(-3.04121518109165,-1.35701590021474,
-0.638439244467571));
#16733=CARTESIAN_POINT('Ctrl Pts',(-3.05853006762437,-1.45995525957164,
-0.318059253537677));
#16734=CARTESIAN_POINT('Ctrl Pts',(-3.07584495415709,-1.46212013789102,
0.00104925812874614));
#16735=CARTESIAN_POINT('Ctrl Pts',(-3.14715504584291,-1.46215854801559,
0.001064531573891));
#16736=CARTESIAN_POINT('Ctrl Pts',(-3.12974812117023,-1.45994645696379,
-0.319718893924214));
#16737=CARTESIAN_POINT('Ctrl Pts',(-3.11234119649755,-1.35582063834627,
-0.641808687614994));
#16738=CARTESIAN_POINT('Ctrl Pts',(-3.09493427182487,-1.16135833267832,
-0.894332644230534));
#16739=CARTESIAN_POINT('Ctrl Pts',(-3.06871073663744,-0.868400833797661,
-1.27476003083089));
#16740=CARTESIAN_POINT('Ctrl Pts',(-3.04248720145001,-0.370420811302354,
-1.49730477288509));
#16741=CARTESIAN_POINT('Ctrl Pts',(-3.01626366626258,0.108419216308635,
-1.46178977272535));
#16742=CARTESIAN_POINT('Ctrl Pts',(-2.99004013107515,0.587259243919631,
-1.42627477256562));
#16743=CARTESIAN_POINT('Ctrl Pts',(-2.96381659588772,1.04695927664631,-1.13270003019193));
#16744=CARTESIAN_POINT('Ctrl Pts',(-2.93759306070029,1.28058832546627,-0.713216352864168));
#16745=CARTESIAN_POINT('Ctrl Pts',(-2.91136952551286,1.51421737428623,-0.293732675536404));
#16746=CARTESIAN_POINT('Ctrl Pts',(-2.88514599032543,1.52177543919947,0.25165993674544));
#16747=CARTESIAN_POINT('Ctrl Pts',(-2.858922455138,1.29986025823381,0.67745655287492));
#16748=CARTESIAN_POINT('Ctrl Pts',(-2.83269891995057,1.07794507726815,1.10325316900439));
#16749=CARTESIAN_POINT('Ctrl Pts',(-2.80647538476314,0.626556650423587,
1.40945378898151));
#16750=CARTESIAN_POINT('Ctrl Pts',(-2.78025184957571,0.14888466646931,1.45822408364331));
#16751=CARTESIAN_POINT('Ctrl Pts',(-2.75402831438828,-0.328787317484966,
1.50699437830511));
#16752=CARTESIAN_POINT('Ctrl Pts',(-2.72780477920085,-0.832742858548961,
1.29833434765159));
#16753=CARTESIAN_POINT('Ctrl Pts',(-2.70158124401342,-1.13612978259562,
0.926171131866864));
#16754=CARTESIAN_POINT('Ctrl Pts',(-2.68343917795658,-1.34602008066168,
0.668699757529504));
#16755=CARTESIAN_POINT('Ctrl Pts',(-2.66529711189975,-1.4599141899931,0.33297245835215));
#16756=CARTESIAN_POINT('Ctrl Pts',(-2.64715504584291,-1.46248673610352,
-0.00116876785021116));
#16757=CARTESIAN_POINT('Origin',(-4.675,0.,0.));
#16758=CARTESIAN_POINT('',(-2.07584495415709,-1.46567283994288,0.000450589203851749));
#16759=CARTESIAN_POINT('',(-2.14715504584291,-1.46566693596749,0.000405098676182412));
#16760=CARTESIAN_POINT('',(-4.675,-1.4635,-1.79227059055215E-16));
#16761=CARTESIAN_POINT('Ctrl Pts',(-2.07584495415709,-1.46567283994288,
0.000450589203851749));
#16762=CARTESIAN_POINT('Ctrl Pts',(-2.07718097870854,-1.46577104663176,
0.0249220526474152));
#16763=CARTESIAN_POINT('Ctrl Pts',(-2.07851700326,-1.46521215258492,0.0493888675234306));
#16764=CARTESIAN_POINT('Ctrl Pts',(-2.07985302781145,-1.46398217331303,
0.0738216850181092));
#16765=CARTESIAN_POINT('Ctrl Pts',(-2.10607656299888,-1.43984009846771,
0.553389855081013));
#16766=CARTESIAN_POINT('Ctrl Pts',(-2.13230009818631,-1.15715592121758,
1.01986020370653));
#16767=CARTESIAN_POINT('Ctrl Pts',(-2.15852363337374,-0.743301695393459,
1.26333911036547));
#16768=CARTESIAN_POINT('Ctrl Pts',(-2.18474716856117,-0.329447469569337,
1.50681801702441));
#16769=CARTESIAN_POINT('Ctrl Pts',(-2.2109707037486,0.215576804828768,1.52730548171678));
#16770=CARTESIAN_POINT('Ctrl Pts',(-2.23719423893603,0.646496882664062,
1.31553455114735));
#16771=CARTESIAN_POINT('Ctrl Pts',(-2.26341777412346,1.07741696049935,1.10376362057792));
#16772=CARTESIAN_POINT('Ctrl Pts',(-2.28964130931089,1.39423284177183,0.659734294746721));
#16773=CARTESIAN_POINT('Ctrl Pts',(-2.31586484449832,1.45429777609794,0.183346983329943));
#16774=CARTESIAN_POINT('Ctrl Pts',(-2.34208837968575,1.51436271042405,-0.293040328086842));
#16775=CARTESIAN_POINT('Ctrl Pts',(-2.36831191487318,1.31767669780378,-0.801785625089211));
#16776=CARTESIAN_POINT('Ctrl Pts',(-2.39453545006061,0.952794611848804,
-1.11389281353731));
#16777=CARTESIAN_POINT('Ctrl Pts',(-2.42075898524804,0.587912525893835,
-1.4260000019854));
#16778=CARTESIAN_POINT('Ctrl Pts',(-2.44698252043547,0.0548343666041687,
-1.54146908187924));
#16779=CARTESIAN_POINT('Ctrl Pts',(-2.4732060556229,-0.406487582422807,
-1.40831590953028));
#16780=CARTESIAN_POINT('Ctrl Pts',(-2.49942959081033,-0.867809531449795,
-1.27516273718131));
#16781=CARTESIAN_POINT('Ctrl Pts',(-2.52565312599776,-1.25737527021408,
-0.893387312589523));
#16782=CARTESIAN_POINT('Ctrl Pts',(-2.55187666118519,-1.39981933451332,
-0.434846793744943));
#16783=CARTESIAN_POINT('Ctrl Pts',(-2.55986609217582,-1.44321725983536,
-0.295144888356011));
#16784=CARTESIAN_POINT('Ctrl Pts',(-2.56785552316646,-1.46367694682157,
-0.148317521262214));
#16785=CARTESIAN_POINT('Ctrl Pts',(-2.57584495415709,-1.46253100424383,
-0.00117902711067597));
#16786=CARTESIAN_POINT('Ctrl Pts',(-2.64715504584291,-1.46248673610352,
-0.00116876785021116));
#16787=CARTESIAN_POINT('Ctrl Pts',(-2.63907357671231,-1.46363268893565,
-0.150013557432222));
#16788=CARTESIAN_POINT('Ctrl Pts',(-2.63099210758172,-1.44268911331045,
-0.298543622686762));
#16789=CARTESIAN_POINT('Ctrl Pts',(-2.62291063845113,-1.39830137570459,
-0.439701606098301));
#16790=CARTESIAN_POINT('Ctrl Pts',(-2.5966871032637,-1.25426773773756,-0.897744727362739));
#16791=CARTESIAN_POINT('Ctrl Pts',(-2.57046356807627,-0.863382154774179,
-1.27816456897568));
#16792=CARTESIAN_POINT('Ctrl Pts',(-2.54424003288884,-0.401599883091991,
-1.4097169734956));
#16793=CARTESIAN_POINT('Ctrl Pts',(-2.51801649770141,0.0601823885902093,
-1.54126937801552));
#16794=CARTESIAN_POINT('Ctrl Pts',(-2.49179296251398,0.592861348991231,
-1.42395434544243));
#16795=CARTESIAN_POINT('Ctrl Pts',(-2.46556942732655,0.956656176813372,
-1.11058164716247));
#16796=CARTESIAN_POINT('Ctrl Pts',(-2.43934589213912,1.32045100463551,-0.797208948882529));
#16797=CARTESIAN_POINT('Ctrl Pts',(-2.41312235695169,1.51536169987877,-0.287778584895738));
#16798=CARTESIAN_POINT('Ctrl Pts',(-2.38689882176426,1.45364820629875,0.188394856012302));
#16799=CARTESIAN_POINT('Ctrl Pts',(-2.36067528657683,1.39193471271873,0.664568296920349));
#16800=CARTESIAN_POINT('Ctrl Pts',(-2.3344517513894,1.07359703031543,1.10748481474964));
#16801=CARTESIAN_POINT('Ctrl Pts',(-2.30822821620197,0.641937119850225,
1.31776417412904));
#16802=CARTESIAN_POINT('Ctrl Pts',(-2.28200468101454,0.21027720938502,1.52804353350844));
#16803=CARTESIAN_POINT('Ctrl Pts',(-2.25578114582711,-0.33470492914208,
1.50568573443795));
#16804=CARTESIAN_POINT('Ctrl Pts',(-2.22955761063968,-0.747697270824022,
1.26076301132885));
#16805=CARTESIAN_POINT('Ctrl Pts',(-2.20333407545225,-1.16068961250596,
1.01584028821975));
#16806=CARTESIAN_POINT('Ctrl Pts',(-2.17711054026482,-1.44169215734274,
0.54835264107206));
#16807=CARTESIAN_POINT('Ctrl Pts',(-2.15088700507739,-1.46419785181459,
0.0687213793496122));
#16808=CARTESIAN_POINT('Ctrl Pts',(-2.14964301866589,-1.46526547209935,
0.0459687349084391));
#16809=CARTESIAN_POINT('Ctrl Pts',(-2.1483990322544,-1.465751385703,0.0231887631643572));
#16810=CARTESIAN_POINT('Ctrl Pts',(-2.14715504584291,-1.46566693596749,
0.000405098676182412));
#16811=CARTESIAN_POINT('Origin',(-8.66086711473615,0.,0.));
#16812=CARTESIAN_POINT('',(-1.91086711473615,-1.17949859053141,0.000362611161451894));
#16813=CARTESIAN_POINT('',(-1.81213288526384,-1.17599517010053,0.000374536726006555));
#16814=CARTESIAN_POINT('',(-8.66086711473615,-1.17775,-9.40918233355216E-14));
#16815=CARTESIAN_POINT('',(-1.6865,1.11895033756726,-0.372858137362636));
#16816=CARTESIAN_POINT('Ctrl Pts',(-1.91086711473615,-1.17949859053141,
0.000362611161451828));
#16817=CARTESIAN_POINT('Ctrl Pts',(-1.88597960410018,-1.17802638490066,
-0.366486395610538));
#16818=CARTESIAN_POINT('Ctrl Pts',(-1.83486855827677,-0.798160605577452,
-1.12254371076134));
#16819=CARTESIAN_POINT('Ctrl Pts',(-1.76007952003139,0.441176614863831,
-1.29467055259558));
#16820=CARTESIAN_POINT('Ctrl Pts',(-1.71017799242198,1.00633421131011,-0.703481264185673));
#16821=CARTESIAN_POINT('Ctrl Pts',(-1.6865,1.11895033756726,-0.372858137362636));
#16822=CARTESIAN_POINT('',(-1.6865,0.00936663037056419,-1.17771275306651));
#16823=CARTESIAN_POINT('Origin',(-1.6865,0.,0.));
#16824=CARTESIAN_POINT('Ctrl Pts',(-1.81213288526384,-1.17599517010053,
0.000374536726006642));
#16825=CARTESIAN_POINT('Ctrl Pts',(-1.79647879202999,-1.17477985141934,
-0.232212701039649));
#16826=CARTESIAN_POINT('Ctrl Pts',(-1.75460116360871,-0.995964068408633,
-0.855730562959772));
#16827=CARTESIAN_POINT('Ctrl Pts',(-1.71272353518743,-0.378730543625381,
-1.1807993824396));
#16828=CARTESIAN_POINT('Ctrl Pts',(-1.6865,0.00936663037056419,-1.17771275306651));
#16829=CARTESIAN_POINT('Origin',(-8.66086711473615,0.,0.));
#16830=CARTESIAN_POINT('',(-2.41086711473615,-1.17697020174115,-0.000948820758233051));
#16831=CARTESIAN_POINT('',(-2.31213288526384,-1.17949383931378,0.000326002709753635));
#16832=CARTESIAN_POINT('',(-8.66086711473615,-1.17775,-9.40918233355216E-14));
#16833=CARTESIAN_POINT('Ctrl Pts',(-2.41086711473615,-1.17697020174115,
-0.000948820758233052));
#16834=CARTESIAN_POINT('Ctrl Pts',(-2.40287768374552,-1.17789239775818,
-0.119358360551166));
#16835=CARTESIAN_POINT('Ctrl Pts',(-2.36866471756746,-1.10738507091887,
-0.625348758528117));
#16836=CARTESIAN_POINT('Ctrl Pts',(-2.30822821620197,-0.384866161144742,
-1.33341914590248));
#16837=CARTESIAN_POINT('Ctrl Pts',(-2.22955761063968,0.902116009207335,
-1.05464830440266));
#16838=CARTESIAN_POINT('Ctrl Pts',(-2.15088700507739,1.37696456000371,0.173588334226353));
#16839=CARTESIAN_POINT('Ctrl Pts',(-2.0722163995151,0.612092873972952,1.24558465502793));
#16840=CARTESIAN_POINT('Ctrl Pts',(-1.9935457939528,-0.703730164986462,
1.19612286163926));
#16841=CARTESIAN_POINT('Ctrl Pts',(-1.93976269902649,-1.1702997645752,0.426214599014237));
#16842=CARTESIAN_POINT('Ctrl Pts',(-1.91220313928761,-1.17957762225525,
0.0200559941957292));
#16843=CARTESIAN_POINT('Ctrl Pts',(-1.91086711473615,-1.17949859053141,
0.000362611161451828));
#16844=CARTESIAN_POINT('Ctrl Pts',(-2.31213288526384,-1.17949383931378,
0.000326002709753667));
#16845=CARTESIAN_POINT('Ctrl Pts',(-2.2871533364879,-1.17812916935092,-0.36784782733973));
#16846=CARTESIAN_POINT('Ctrl Pts',(-2.23595025252454,-0.795963231226945,
-1.12498678959492));
#16847=CARTESIAN_POINT('Ctrl Pts',(-2.15852363337374,0.488222034063068,
-1.29907078650092));
#16848=CARTESIAN_POINT('Ctrl Pts',(-2.07985302781145,1.35367817671458,-0.306589740084279));
#16849=CARTESIAN_POINT('Ctrl Pts',(-2.00118242224916,1.00009581383204,0.962242750523822));
#16850=CARTESIAN_POINT('Ctrl Pts',(-1.92251181668687,-0.253212907927416,
1.36414589400647));
#16851=CARTESIAN_POINT('Ctrl Pts',(-1.85949530435843,-1.07552588043857,
0.703308252629748));
#16852=CARTESIAN_POINT('Ctrl Pts',(-1.82270232721742,-1.17681573760732,
0.157414441368478));
#16853=CARTESIAN_POINT('Ctrl Pts',(-1.81213288526384,-1.17599517010053,
0.000374536726006642));
#16854=CARTESIAN_POINT('Origin',(-8.66086711473615,0.,0.));
#16855=CARTESIAN_POINT('',(-2.91086711473616,-1.17663955749993,0.000844389314044513));
#16856=CARTESIAN_POINT('',(-2.81213288526384,-1.17693457700439,-0.000940564629799273));
#16857=CARTESIAN_POINT('',(-8.66086711473615,-1.17775,-9.40918233355216E-14));
#16858=CARTESIAN_POINT('Ctrl Pts',(-2.91086711473616,-1.17663955749993,
0.000844389314044337));
#16859=CARTESIAN_POINT('Ctrl Pts',(-2.89355222820344,-1.17489737407618,
-0.255957831126769));
#16860=CARTESIAN_POINT('Ctrl Pts',(-2.85001380648329,-0.966594683781144,
-0.904261982661384));
#16861=CARTESIAN_POINT('Ctrl Pts',(-2.78025184957571,0.0978503055697247,
-1.38439494624008));
#16862=CARTESIAN_POINT('Ctrl Pts',(-2.70158124401342,1.21013193153834,-0.679488016032942));
#16863=CARTESIAN_POINT('Ctrl Pts',(-2.62291063845113,1.232947968949,0.637152805391334));
#16864=CARTESIAN_POINT('Ctrl Pts',(-2.54424003288884,0.145755609165987,
1.38017397139449));
#16865=CARTESIAN_POINT('Ctrl Pts',(-2.47355885831718,-0.948919964424747,
0.931371035446015));
#16866=CARTESIAN_POINT('Ctrl Pts',(-2.42910121893295,-1.17486549387346,
0.269294690827376));
#16867=CARTESIAN_POINT('Ctrl Pts',(-2.41086711473615,-1.17697020174115,
-0.000948820758233052));
#16868=CARTESIAN_POINT('Ctrl Pts',(-2.81213288526384,-1.17693457700439,
-0.000940564629799308));
#16869=CARTESIAN_POINT('Ctrl Pts',(-2.80405141613325,-1.17785678127362,
-0.120723243775803));
#16870=CARTESIAN_POINT('Ctrl Pts',(-2.76974641181523,-1.10631193161732,
-0.62811326056394));
#16871=CARTESIAN_POINT('Ctrl Pts',(-2.70921787230977,-0.38024109152726,
-1.33474396280885));
#16872=CARTESIAN_POINT('Ctrl Pts',(-2.63054726674748,0.905777314237609,
-1.05151653620214));
#16873=CARTESIAN_POINT('Ctrl Pts',(-2.5518766611852,1.37633981097026,0.178374023112081));
#16874=CARTESIAN_POINT('Ctrl Pts',(-2.4732060556229,0.607794121628612,1.24768375090184));
#16875=CARTESIAN_POINT('Ctrl Pts',(-2.39453545006062,-0.707927190944584,
1.19370650897096));
#16876=CARTESIAN_POINT('Ctrl Pts',(-2.34084439327426,-1.17092757672768,
0.423439602299549));
#16877=CARTESIAN_POINT('Ctrl Pts',(-2.31337687167533,-1.17956180014466,
0.018661131408755));
#16878=CARTESIAN_POINT('Ctrl Pts',(-2.31213288526384,-1.17949383931378,
0.000326002709753667));
#16879=CARTESIAN_POINT('Origin',(-8.66086711473615,0.,0.));
#16880=CARTESIAN_POINT('',(-3.41086711473615,-1.17959136717079,-0.000110183320623983));
#16881=CARTESIAN_POINT('',(-3.31213288526384,-1.17667046800503,0.000856680601965393));
#16882=CARTESIAN_POINT('',(-8.66086711473615,-1.17775,-9.40918233355216E-14));
#16883=CARTESIAN_POINT('Ctrl Pts',(-3.41086711473615,-1.17959136717079,
-0.000110183320623943));
#16884=CARTESIAN_POINT('Ctrl Pts',(-3.41045030784878,-1.17959970513283,
-0.00625203394745172));
#16885=CARTESIAN_POINT('Ctrl Pts',(-3.38380996577397,-1.1767938832024,-0.398802509579523));
#16886=CARTESIAN_POINT('Ctrl Pts',(-3.33094608851175,-0.744809034162001,
-1.17106078215508));
#16887=CARTESIAN_POINT('Ctrl Pts',(-3.25227548294945,0.568601241925253,
-1.26602388853876));
#16888=CARTESIAN_POINT('Ctrl Pts',(-3.17360487738716,1.37010712465924,-0.22120196322891));
#16889=CARTESIAN_POINT('Ctrl Pts',(-3.09493427182487,0.938123194652226,
1.02276523601594));
#16890=CARTESIAN_POINT('Ctrl Pts',(-3.01626366626258,-0.338441009250009,
1.34595006244152));
#16891=CARTESIAN_POINT('Ctrl Pts',(-2.95490794723301,-1.09640882153771,
0.652958858257086));
#16892=CARTESIAN_POINT('Ctrl Pts',(-2.91977576339087,-1.17753592491099,
0.132971201195474));
#16893=CARTESIAN_POINT('Ctrl Pts',(-2.91086711473616,-1.17663955749993,
0.000844389314044337));
#16894=CARTESIAN_POINT('Ctrl Pts',(-3.31213288526384,-1.17667046800503,
0.000856680601965358));
#16895=CARTESIAN_POINT('Ctrl Pts',(-3.29472596059116,-1.17489029018727,
-0.257293424885117));
#16896=CARTESIAN_POINT('Ctrl Pts',(-3.25109550073105,-0.964857764256308,
-0.906981790783454));
#16897=CARTESIAN_POINT('Ctrl Pts',(-3.18124150568352,0.102653133571944,
-1.38404698750922));
#16898=CARTESIAN_POINT('Ctrl Pts',(-3.10257090012123,1.2124824062959,-0.675285143647363));
#16899=CARTESIAN_POINT('Ctrl Pts',(-3.02390029455893,1.23072943933634,0.641427153820911));
#16900=CARTESIAN_POINT('Ctrl Pts',(-2.94522968899665,0.140966433426828,
1.38067098062933));
#16901=CARTESIAN_POINT('Ctrl Pts',(-2.87464055256494,-0.950723338242491,
0.928662811933087));
#16902=CARTESIAN_POINT('Ctrl Pts',(-2.83027495132068,-1.17486432337848,
0.267959216142224));
#16903=CARTESIAN_POINT('Ctrl Pts',(-2.81213288526384,-1.17693457700439,
-0.000940564629799308));
#16904=CARTESIAN_POINT('Origin',(-8.66086711473615,0.,0.));
#16905=CARTESIAN_POINT('',(-3.91086711473616,-1.17638334390667,-0.000716697455210677));
#16906=CARTESIAN_POINT('',(-3.81213288526384,-1.17958479253191,-0.000134358022525483));
#16907=CARTESIAN_POINT('',(-8.66086711473615,-1.17775,-9.40918233355216E-14));
#16908=CARTESIAN_POINT('Ctrl Pts',(-3.91086711473616,-1.17638334390667,
-0.000716697455210805));
#16909=CARTESIAN_POINT('Ctrl Pts',(-3.9011248523067,-1.17720337900645,-0.145286422711667));
#16910=CARTESIAN_POINT('Ctrl Pts',(-3.86515905468981,-1.08593957103214,
-0.677999935594477));
#16911=CARTESIAN_POINT('Ctrl Pts',(-3.80296972188548,-0.295982347342492,
-1.35591972587991));
#16912=CARTESIAN_POINT('Ctrl Pts',(-3.72429911632319,0.969796609117977,
-0.992783153602477));
#16913=CARTESIAN_POINT('Ctrl Pts',(-3.6456285107609,1.36248014896398,0.264143325656574));
#16914=CARTESIAN_POINT('Ctrl Pts',(-3.56695790519861,0.528540331258045,
1.28326496528333));
#16915=CARTESIAN_POINT('Ctrl Pts',(-3.4887041065237,-0.774298180626516,
1.14780118577342));
#16916=CARTESIAN_POINT('Ctrl Pts',(-3.43667384303621,-1.17907511965292,
0.380164411911229));
#16917=CARTESIAN_POINT('Ctrl Pts',(-3.41086711473615,-1.17959136717079,
-0.000110183320623943));
#16918=CARTESIAN_POINT('Ctrl Pts',(-3.81213288526384,-1.17958479253191,
-0.000134358022525584));
#16919=CARTESIAN_POINT('Ctrl Pts',(-3.8116240402365,-1.17959709699341,-0.00763254663005804));
#16920=CARTESIAN_POINT('Ctrl Pts',(-3.78489166002174,-1.17615977017934,
-0.401541357004618));
#16921=CARTESIAN_POINT('Ctrl Pts',(-3.73193574461955,-0.740741232249389,
-1.17363798581818));
#16922=CARTESIAN_POINT('Ctrl Pts',(-3.65326513905726,0.572990579286003,
-1.26404331095425));
#16923=CARTESIAN_POINT('Ctrl Pts',(-3.57459453349497,1.3708663395606,-0.216446696849244));
#16924=CARTESIAN_POINT('Ctrl Pts',(-3.49592392793268,0.934568764120381,
1.02601409348018));
#16925=CARTESIAN_POINT('Ctrl Pts',(-3.41725332237039,-0.34310905511451,
1.34476759219195));
#16926=CARTESIAN_POINT('Ctrl Pts',(-3.35598964148077,-1.09753440075601,
0.65019412424173));
#16927=CARTESIAN_POINT('Ctrl Pts',(-3.32094949577859,-1.17757212839372,
0.131609756014222));
#16928=CARTESIAN_POINT('Ctrl Pts',(-3.31213288526384,-1.17667046800503,
0.000856680601965358));
#16929=CARTESIAN_POINT('Origin',(-8.66086711473615,0.,0.));
#16930=CARTESIAN_POINT('',(-4.41086711473616,-1.17730203530188,0.00100741500783658));
#16931=CARTESIAN_POINT('',(-4.31213288526384,-1.17635786578603,-0.000700921021541262));
#16932=CARTESIAN_POINT('',(-8.66086711473615,-1.17775,-9.40918233355216E-14));
#16933=CARTESIAN_POINT('Ctrl Pts',(-4.41086711473616,-1.17730203530188,
0.00100741500783666));
#16934=CARTESIAN_POINT('Ctrl Pts',(-4.39179939676461,-1.17491412509447,
-0.28138822708182));
#16935=CARTESIAN_POINT('Ctrl Pts',(-4.34650814360563,-0.932258082234428,
-0.955843334036929));
#16936=CARTESIAN_POINT('Ctrl Pts',(-4.27499335525923,0.189051166264626,
-1.37491218247906));
#16937=CARTESIAN_POINT('Ctrl Pts',(-4.19632274969693,1.25235902888845,-0.598097580467343));
#16938=CARTESIAN_POINT('Ctrl Pts',(-4.11765214413465,1.18818416202297,0.717176582238888));
#16939=CARTESIAN_POINT('Ctrl Pts',(-4.03898153857235,0.0543023730844936,
1.38678589020371));
#16940=CARTESIAN_POINT('Ctrl Pts',(-3.97005319543952,-0.981997558039448,
0.879577951977616));
#16941=CARTESIAN_POINT('Ctrl Pts',(-3.92734838749413,-1.17499606633655,
0.243856171706187));
#16942=CARTESIAN_POINT('Ctrl Pts',(-3.91086711473616,-1.17638334390667,
-0.000716697455210805));
#16943=CARTESIAN_POINT('Ctrl Pts',(-4.31213288526384,-1.17635786578603,
-0.000700921021541401));
#16944=CARTESIAN_POINT('Ctrl Pts',(-4.30229858469442,-1.17716630005596,
-0.146644373245256));
#16945=CARTESIAN_POINT('Ctrl Pts',(-4.26624074893757,-1.08475308443882,
-0.680764528174929));
#16946=CARTESIAN_POINT('Ctrl Pts',(-4.20395937799329,-0.29127585234018,
-1.35693849265711));
#16947=CARTESIAN_POINT('Ctrl Pts',(-4.125288772431,0.973235439907126,-0.989412185868934));
#16948=CARTESIAN_POINT('Ctrl Pts',(-4.04661816686871,1.36155538052876,0.268869188915402));
#16949=CARTESIAN_POINT('Ctrl Pts',(-3.96794756130642,0.524084520485498,
1.28509109030307));
#16950=CARTESIAN_POINT('Ctrl Pts',(-3.88978580077146,-0.776744299388545,
1.14527225033765));
#16951=CARTESIAN_POINT('Ctrl Pts',(-3.83784757542394,-1.1789629815715,0.378789649184804));
#16952=CARTESIAN_POINT('Ctrl Pts',(-3.81213288526384,-1.17958479253191,
-0.000134358022525584));
#16953=CARTESIAN_POINT('Origin',(-8.66086711473615,0.,0.));
#16954=CARTESIAN_POINT('',(-4.91086711473616,-1.17927992659326,-0.000541138395992998));
#16955=CARTESIAN_POINT('',(-4.81213288526384,-1.1773401869437,0.00101152320117252));
#16956=CARTESIAN_POINT('',(-8.66086711473615,-1.17775,-9.40918233355216E-14));
#16957=CARTESIAN_POINT('Ctrl Pts',(-4.91086711473616,-1.17927992659326,
-0.000541138395993047));
#16958=CARTESIAN_POINT('Ctrl Pts',(-4.90869747640996,-1.1794645160417,-0.0325343443996988));
#16959=CARTESIAN_POINT('Ctrl Pts',(-4.88030430289632,-1.16387484001231,
-0.451033884711238));
#16960=CARTESIAN_POINT('Ctrl Pts',(-4.82568759419526,-0.66585587424462,
-1.21768625176223));
#16961=CARTESIAN_POINT('Ctrl Pts',(-4.74701698863296,0.650958493169218,
-1.22571484985989));
#16962=CARTESIAN_POINT('Ctrl Pts',(-4.66834638307068,1.38172329992943,-0.130248130230639));
#16963=CARTESIAN_POINT('Ctrl Pts',(-4.58967577750838,0.868540387494536,
1.08247930617046));
#16964=CARTESIAN_POINT('Ctrl Pts',(-4.5110051719461,-0.42657826714551,1.32066454294621));
#16965=CARTESIAN_POINT('Ctrl Pts',(-4.45140228435535,-1.1168328254269,0.60031985529612));
#16966=CARTESIAN_POINT('Ctrl Pts',(-4.41802293195204,-1.17819818076604,
0.106986095853185));
#16967=CARTESIAN_POINT('Ctrl Pts',(-4.41086711473616,-1.17730203530188,
0.00100741500783666));
#16968=CARTESIAN_POINT('Ctrl Pts',(-4.81213288526384,-1.1773401869437,0.00101152320117258));
#16969=CARTESIAN_POINT('Ctrl Pts',(-4.79297312915233,-1.17492446024765,
-0.282723747894919));
#16970=CARTESIAN_POINT('Ctrl Pts',(-4.7475898378534,-0.930380861478271,
-0.958537919647446));
#16971=CARTESIAN_POINT('Ctrl Pts',(-4.67598301136704,0.193820620708426,
-1.37424788957624));
#16972=CARTESIAN_POINT('Ctrl Pts',(-4.59731240580474,1.25442668732974,-0.593748584109574));
#16973=CARTESIAN_POINT('Ctrl Pts',(-4.51864180024246,1.18568853815801,0.721294936553209));
#16974=CARTESIAN_POINT('Ctrl Pts',(-4.43997119468016,0.049490244982279,
1.38696590104707));
#16975=CARTESIAN_POINT('Ctrl Pts',(-4.37113488968729,-0.983662136505136,
0.876847394213616));
#16976=CARTESIAN_POINT('Ctrl Pts',(-4.32852211988185,-1.1750105794356,0.242519373352494));
#16977=CARTESIAN_POINT('Ctrl Pts',(-4.31213288526384,-1.17635786578603,
-0.000700921021541401));
#16978=CARTESIAN_POINT('Origin',(-8.66086711473615,0.,0.));
#16979=CARTESIAN_POINT('',(-5.41086711473616,-1.17600992997557,-0.000371065616479655));
#16980=CARTESIAN_POINT('',(-5.31213288526384,-1.17925411379821,-0.000561242925713745));
#16981=CARTESIAN_POINT('',(-8.66086711473615,-1.17775,-9.40918233355216E-14));
#16982=CARTESIAN_POINT('Ctrl Pts',(-5.41086711473616,-1.17600992997557,
-0.000371065616479732));
#16983=CARTESIAN_POINT('Ctrl Pts',(-5.39937202086787,-1.17650112810648,
-0.171087869735001));
#16984=CARTESIAN_POINT('Ctrl Pts',(-5.36165339181215,-1.06227811533873,
-0.730631560415982));
#16985=CARTESIAN_POINT('Ctrl Pts',(-5.297711227569,-0.205802127560476,-1.37250476768144));
#16986=CARTESIAN_POINT('Ctrl Pts',(-5.21904062200671,1.03323559121881,-0.926578688525379));
#16987=CARTESIAN_POINT('Ctrl Pts',(-5.14037001644442,1.34206459371129,0.353534268919763));
#16988=CARTESIAN_POINT('Ctrl Pts',(-5.06169941088212,0.442650100242435,
1.31536487019939));
#16989=CARTESIAN_POINT('Ctrl Pts',(-4.98519844364604,-0.819481368292237,
1.09912223479354));
#16990=CARTESIAN_POINT('Ctrl Pts',(-4.93492101159739,-1.17723345852483,
0.354154512109054));
#16991=CARTESIAN_POINT('Ctrl Pts',(-4.91086711473616,-1.17927992659326,
-0.000541138395993047));
#16992=CARTESIAN_POINT('Ctrl Pts',(-5.31213288526384,-1.17925411379821,
-0.000561242925713546));
#16993=CARTESIAN_POINT('Ctrl Pts',(-5.30987120879768,-1.17945240900491,
-0.0339135600639547));
#16994=CARTESIAN_POINT('Ctrl Pts',(-5.28138599714409,-1.16314653333968,
-0.45378048918944));
#16995=CARTESIAN_POINT('Ctrl Pts',(-5.22667725030306,-0.66162677306598,
-1.21998922461717));
#16996=CARTESIAN_POINT('Ctrl Pts',(-5.14800664474078,0.655207470874117,
-1.22344875868442));
#16997=CARTESIAN_POINT('Ctrl Pts',(-5.06933603917847,1.38216685417029,-0.12545310777169));
#16998=CARTESIAN_POINT('Ctrl Pts',(-4.9906654336162,0.86477919209241,1.08548636285362));
#16999=CARTESIAN_POINT('Ctrl Pts',(-4.9119948280539,-0.431158056335988,
1.31917641938943));
#17000=CARTESIAN_POINT('Ctrl Pts',(-4.85248397860312,-1.11784699831804,
0.597557127533712));
#17001=CARTESIAN_POINT('Ctrl Pts',(-4.81919666433976,-1.17823081204297,
0.105618453446316));
#17002=CARTESIAN_POINT('Ctrl Pts',(-4.81213288526384,-1.1773401869437,0.00101152320117258));
#17003=CARTESIAN_POINT('Origin',(-8.66086711473615,0.,0.));
#17004=CARTESIAN_POINT('',(-5.91086711473616,-1.1780553849581,0.00100231958302903));
#17005=CARTESIAN_POINT('',(-5.81213288526384,-1.17599715609266,-0.000350803616455952));
#17006=CARTESIAN_POINT('',(-8.66086711473615,-1.17775,-9.40918233355216E-14));
#17007=CARTESIAN_POINT('Ctrl Pts',(-5.91086711473616,-1.1780553849581,0.00100231958302903));
#17008=CARTESIAN_POINT('Ctrl Pts',(-5.89004656532578,-1.17529941481109,
-0.306848134423301));
#17009=CARTESIAN_POINT('Ctrl Pts',(-5.84300248072798,-0.895208689127834,
-1.0068819708241));
#17010=CARTESIAN_POINT('Ctrl Pts',(-5.76973486094274,0.279426911638065,
-1.3594279881432));
#17011=CARTESIAN_POINT('Ctrl Pts',(-5.69106425538045,1.28911939778457,-0.514096324773416));
#17012=CARTESIAN_POINT('Ctrl Pts',(-5.61239364981816,1.13823426692583,0.794069648334226));
#17013=CARTESIAN_POINT('Ctrl Pts',(-5.53372304425587,-0.0373885377105224,
1.38734492840875));
#17014=CARTESIAN_POINT('Ctrl Pts',(-5.46654753256187,-1.01249108072428,
0.827425065489171));
#17015=CARTESIAN_POINT('Ctrl Pts',(-5.4255955560553,-1.17538056731615,0.218365071770556));
#17016=CARTESIAN_POINT('Ctrl Pts',(-5.41086711473616,-1.17600992997557,
-0.000371065616479732));
#17017=CARTESIAN_POINT('Ctrl Pts',(-5.81213288526384,-1.17599715609266,
-0.000350803616455952));
#17018=CARTESIAN_POINT('Ctrl Pts',(-5.80054575325559,-1.17646494966617,
-0.172439149737962));
#17019=CARTESIAN_POINT('Ctrl Pts',(-5.76273508605991,-1.06097257609266,
-0.733393343710012));
#17020=CARTESIAN_POINT('Ctrl Pts',(-5.69870088367681,-0.201038633207167,
-1.37321053124158));
#17021=CARTESIAN_POINT('Ctrl Pts',(-5.62003027811452,1.03644432469548,-0.922988004686612));
#17022=CARTESIAN_POINT('Ctrl Pts',(-5.54135967255223,1.34082978479473,0.358188753595292));
#17023=CARTESIAN_POINT('Ctrl Pts',(-5.46268906698994,0.438083431536926,
1.31689278305031));
#17024=CARTESIAN_POINT('Ctrl Pts',(-5.3862801378938,-0.821772524436675,
1.09653760690973));
#17025=CARTESIAN_POINT('Ctrl Pts',(-5.33609474398511,-1.17715322899035,
0.352797658424898));
#17026=CARTESIAN_POINT('Ctrl Pts',(-5.31213288526384,-1.17925411379821,
-0.000561242925713546));
#17027=CARTESIAN_POINT('Origin',(-8.66086711473615,0.,0.));
#17028=CARTESIAN_POINT('',(-6.41086711473616,-1.17867790410982,-0.000859279010538999));
#17029=CARTESIAN_POINT('',(-6.31213288526384,-1.17809532958918,0.000997103128024986));
#17030=CARTESIAN_POINT('',(-8.66086711473615,-1.17775,-9.40918233355216E-14));
#17031=CARTESIAN_POINT('Ctrl Pts',(-6.41086711473616,-1.17867790410982,
-0.000859279010538855));
#17032=CARTESIAN_POINT('Ctrl Pts',(-6.40694464497113,-1.17915438960473,
-0.0587771547817094));
#17033=CARTESIAN_POINT('Ctrl Pts',(-6.37679864001867,-1.14912484901267,
-0.503407322287921));
#17034=CARTESIAN_POINT('Ctrl Pts',(-6.32042909987877,-0.583996247497372,
-1.25899648606665));
#17035=CARTESIAN_POINT('Ctrl Pts',(-6.24175849431649,0.73047430811023,-1.18005558026704));
#17036=CARTESIAN_POINT('Ctrl Pts',(-6.1630878887542,1.38730824708363,-0.0387257526847742));
#17037=CARTESIAN_POINT('Ctrl Pts',(-6.0844172831919,0.795166405654621,1.1374683419316));
#17038=CARTESIAN_POINT('Ctrl Pts',(-6.00574667762961,-0.512853522972119,
1.28961433097063));
#17039=CARTESIAN_POINT('Ctrl Pts',(-5.9478966214777,-1.13517951613434,0.547741260286263));
#17040=CARTESIAN_POINT('Ctrl Pts',(-5.91627010051321,-1.17877056625389,
0.0808902990821281));
#17041=CARTESIAN_POINT('Ctrl Pts',(-5.91086711473616,-1.1780553849581,0.00100231958302903));
#17042=CARTESIAN_POINT('Ctrl Pts',(-6.31213288526384,-1.17809532958918,
0.000997103128024977));
#17043=CARTESIAN_POINT('Ctrl Pts',(-6.2912202977135,-1.17533124755718,-0.308187145896592));
#17044=CARTESIAN_POINT('Ctrl Pts',(-6.24408417497574,-0.89318672921757,
-1.00954427203146));
#17045=CARTESIAN_POINT('Ctrl Pts',(-6.17072451705056,0.284142091338451,
-1.35845020984985));
#17046=CARTESIAN_POINT('Ctrl Pts',(-6.09205391148824,1.29089537055166,-0.509620287250948));
#17047=CARTESIAN_POINT('Ctrl Pts',(-6.01338330592598,1.13547214593956,0.798014222500227));
#17048=CARTESIAN_POINT('Ctrl Pts',(-5.93471270036367,-0.0422020497217742,
1.38720679169256));
#17049=CARTESIAN_POINT('Ctrl Pts',(-5.86762922680964,-1.01402256959767,
0.824678746007463));
#17050=CARTESIAN_POINT('Ctrl Pts',(-5.82676928844302,-1.17540625790132,
0.217024334120822));
#17051=CARTESIAN_POINT('Ctrl Pts',(-5.81213288526384,-1.17599715609266,
-0.000350803616455952));
#17052=CARTESIAN_POINT('Origin',(-8.66086711473615,0.,0.));
#17053=CARTESIAN_POINT('',(-6.91086711473616,-1.17589437083333,3.29986289264394E-5));
#17054=CARTESIAN_POINT('',(-6.81213288526384,-1.17864116107843,-0.000871798980908167));
#17055=CARTESIAN_POINT('',(-8.66086711473615,-1.17775,-9.40918233355216E-14));
#17056=CARTESIAN_POINT('Ctrl Pts',(-6.91086711473616,-1.17589467053987,
3.29932992490858E-5));
#17057=CARTESIAN_POINT('Ctrl Pts',(-6.89761918942904,-1.17584631531485,
-0.196764413629324));
#17058=CARTESIAN_POINT('Ctrl Pts',(-6.8581477289345,-1.03630390526793,-0.783176720222471));
#17059=CARTESIAN_POINT('Ctrl Pts',(-6.79245273325251,-0.114723332390545,
-1.38309735453967));
#17060=CARTESIAN_POINT('Ctrl Pts',(-6.71378212769023,1.09216436667117,-0.856330476563782));
#17061=CARTESIAN_POINT('Ctrl Pts',(-6.63511152212794,1.31579099157645,0.441382439659493));
#17062=CARTESIAN_POINT('Ctrl Pts',(-6.55644091656565,0.354827664455788,
1.34172299085838));
#17063=CARTESIAN_POINT('Ctrl Pts',(-6.48169278076838,-0.861741836051922,
1.04946482550319));
#17064=CARTESIAN_POINT('Ctrl Pts',(-6.43316818015856,-1.1759688624011,0.32843078925572));
#17065=CARTESIAN_POINT('Ctrl Pts',(-6.41086711473616,-1.17867790410982,
-0.000859279010538855));
#17066=CARTESIAN_POINT('Ctrl Pts',(-6.81213288526384,-1.17864116107843,
-0.000871798980908263));
#17067=CARTESIAN_POINT('Ctrl Pts',(-6.80811837735885,-1.17913357190592,
-0.0601535095849911));
#17068=CARTESIAN_POINT('Ctrl Pts',(-6.77788033426643,-1.14829825666904,
-0.506161144387834));
#17069=CARTESIAN_POINT('Ctrl Pts',(-6.72141875598658,-0.579624239257938,
-1.26101500289363));
#17070=CARTESIAN_POINT('Ctrl Pts',(-6.64274815042429,0.734564342461029,
-1.17751395698303));
#17071=CARTESIAN_POINT('Ctrl Pts',(-6.564077544862,1.38743422631486,-0.0339118586638691));
#17072=CARTESIAN_POINT('Ctrl Pts',(-6.4854069392997,0.791214847056285,1.14022045088028));
#17073=CARTESIAN_POINT('Ctrl Pts',(-6.40673633373742,-0.517325047723218,
1.28782705533921));
#17074=CARTESIAN_POINT('Ctrl Pts',(-6.34897831572546,-1.1360871562569,0.544982882691587));
#17075=CARTESIAN_POINT('Ctrl Pts',(-6.31744383290093,-1.17879729413093,
0.0795173413736451));
#17076=CARTESIAN_POINT('Ctrl Pts',(-6.31213288526384,-1.17809532958918,
0.000997103128024977));
#17077=CARTESIAN_POINT('Origin',(-8.66086711473615,0.,0.));
#17078=CARTESIAN_POINT('',(-7.41086711473616,-1.17877062515776,0.000899836917228718));
#17079=CARTESIAN_POINT('',(-7.31213288526384,-1.17589382943587,6.0515499218719E-5));
#17080=CARTESIAN_POINT('',(-8.66086711473615,-1.17775,-9.40918233355216E-14));
#17081=CARTESIAN_POINT('Ctrl Pts',(-7.41086711473616,-1.17877062515776,
0.00089983691722877));
#17082=CARTESIAN_POINT('Ctrl Pts',(-7.38829373388695,-1.17611490904963,
-0.33232246422372));
#17083=CARTESIAN_POINT('Ctrl Pts',(-7.33949681785032,-0.855386430900654,
-1.05736004564147));
#17084=CARTESIAN_POINT('Ctrl Pts',(-7.26447636662626,0.368594759353147,
-1.33794018873242));
#17085=CARTESIAN_POINT('Ctrl Pts',(-7.18580576106397,1.32024655518524,-0.427887663681729));
#17086=CARTESIAN_POINT('Ctrl Pts',(-7.10713515550168,1.0833192355362,0.867515846081762));
#17087=CARTESIAN_POINT('Ctrl Pts',(-7.02846454993939,-0.128917960242522,
1.38183808732227));
#17088=CARTESIAN_POINT('Ctrl Pts',(-6.96304186968421,-1.04049409675069,
0.775023379664861));
#17089=CARTESIAN_POINT('Ctrl Pts',(-6.92384272461647,-1.17594203180746,
0.192785165323541));
#17090=CARTESIAN_POINT('Ctrl Pts',(-6.91086711473616,-1.17589467053987,
3.29932992490858E-5));
#17091=CARTESIAN_POINT('Ctrl Pts',(-7.31213288526384,-1.17589382943587,
6.05154992187017E-5));
#17092=CARTESIAN_POINT('Ctrl Pts',(-7.29879292181676,-1.17581348019214,
-0.198106859471453));
#17093=CARTESIAN_POINT('Ctrl Pts',(-7.25922942318226,-1.03487877075373,
-0.785943419169282));
#17094=CARTESIAN_POINT('Ctrl Pts',(-7.19344238936034,-0.109920457047265,
-1.38347881456886));
#17095=CARTESIAN_POINT('Ctrl Pts',(-7.11477178379802,1.095127328248,-0.852540070304724));
#17096=CARTESIAN_POINT('Ctrl Pts',(-7.03610117823576,1.31425240912282,0.445947499710114));
#17097=CARTESIAN_POINT('Ctrl Pts',(-6.95743057267344,0.350169610287078,
1.34294482869753));
#17098=CARTESIAN_POINT('Ctrl Pts',(-6.88277447501615,-0.863881069525856,
1.04683402745875));
#17099=CARTESIAN_POINT('Ctrl Pts',(-6.83434191254628,-1.17591704998917,
0.327085987954644));
#17100=CARTESIAN_POINT('Ctrl Pts',(-6.81213288526384,-1.17864116107843,
-0.000871798980908263));
#17101=CARTESIAN_POINT('Origin',(-1.6865,3.28582941601228E-17,0.));
#17102=CARTESIAN_POINT('',(-1.6865,-0.26238990830909,1.43978602091337));
#17103=CARTESIAN_POINT('Ctrl Pts',(-1.6865,1.11895033756726,-0.372858137362636));
#17104=CARTESIAN_POINT('Ctrl Pts',(-1.6865,1.13535536132518,-0.338481041248113));
#17105=CARTESIAN_POINT('Ctrl Pts',(-1.6865,1.14996080409863,-0.303357275824646));
#17106=CARTESIAN_POINT('Ctrl Pts',(-1.6865,1.16267058779846,-0.267595343165902));
#17107=CARTESIAN_POINT('Ctrl Pts',(-1.6865,1.17888071541452,-0.221984378739937));
#17108=CARTESIAN_POINT('Ctrl Pts',(-1.6865,1.19200950533875,-0.175335963428926));
#17109=CARTESIAN_POINT('Ctrl Pts',(-1.6865,1.20217294148064,-0.127929909118842));
#17110=CARTESIAN_POINT('Ctrl Pts',(-1.6865,1.20592469774747,-0.110430319525292));
#17111=CARTESIAN_POINT('Ctrl Pts',(-1.6865,1.2092719382956,-0.0928272229185943));
#17112=CARTESIAN_POINT('Ctrl Pts',(-1.6865,1.21221895595122,-0.0751338976379057));
#17113=CARTESIAN_POINT('Ctrl Pts',(-1.6865,1.21398506969953,-0.0645304915225663));
#17114=CARTESIAN_POINT('Ctrl Pts',(-1.6865,1.21560669230278,-0.0538986526621468));
#17115=CARTESIAN_POINT('Ctrl Pts',(-1.6865,1.21708402895976,-0.0432493233469738));
#17116=CARTESIAN_POINT('Ctrl Pts',(-1.6865,1.22403289104792,0.00684130453578788));
#17117=CARTESIAN_POINT('Ctrl Pts',(-1.6865,1.22780217473515,0.0573687104521416));
#17118=CARTESIAN_POINT('Ctrl Pts',(-1.6865,1.22852178751262,0.108025567468149));
#17119=CARTESIAN_POINT('Ctrl Pts',(-1.6865,1.2290363948802,0.144251149690937));
#17120=CARTESIAN_POINT('Ctrl Pts',(-1.6865,1.22799041925717,0.180543667430809));
#17121=CARTESIAN_POINT('Ctrl Pts',(-1.6865,1.22541633213672,0.216796772140719));
#17122=CARTESIAN_POINT('Ctrl Pts',(-1.6865,1.22459563153091,0.228355411613986));
#17123=CARTESIAN_POINT('Ctrl Pts',(-1.6865,1.22361949764788,0.239910068294751));
#17124=CARTESIAN_POINT('Ctrl Pts',(-1.6865,1.22248871598296,0.251457345648952));
#17125=CARTESIAN_POINT('Ctrl Pts',(-1.6865,1.22157697590322,0.26076782166951));
#17126=CARTESIAN_POINT('Ctrl Pts',(-1.6865,1.22056477417449,0.270071996499609));
#17127=CARTESIAN_POINT('Ctrl Pts',(-1.6865,1.21945390680089,0.279358560962091));
#17128=CARTESIAN_POINT('Ctrl Pts',(-1.6865,1.21322430593567,0.331436415965335));
#17129=CARTESIAN_POINT('Ctrl Pts',(-1.6865,1.20388812344957,0.383041243620923));
#17130=CARTESIAN_POINT('Ctrl Pts',(-1.6865,1.1915757568237,0.433859467629619));
#17131=CARTESIAN_POINT('Ctrl Pts',(-1.6865,1.17901846548233,0.485688597131582));
#17132=CARTESIAN_POINT('Ctrl Pts',(-1.6865,1.16336550530721,0.536700681103785));
#17133=CARTESIAN_POINT('Ctrl Pts',(-1.6865,1.14470297529775,0.586573510429021));
#17134=CARTESIAN_POINT('Ctrl Pts',(-1.6865,1.13355797389477,0.616356865232393));
#17135=CARTESIAN_POINT('Ctrl Pts',(-1.6865,1.12133866272013,0.645734045864069));
#17136=CARTESIAN_POINT('Ctrl Pts',(-1.6865,1.10805456343179,0.674635440120251));
#17137=CARTESIAN_POINT('Ctrl Pts',(-1.6865,1.10137874179942,0.689159612876959));
#17138=CARTESIAN_POINT('Ctrl Pts',(-1.6865,1.09443390630556,0.703563601099449));
#17139=CARTESIAN_POINT('Ctrl Pts',(-1.6865,1.08722064460436,0.717838352010837));
#17140=CARTESIAN_POINT('Ctrl Pts',(-1.6865,1.08181939494862,0.728527204937547));
#17141=CARTESIAN_POINT('Ctrl Pts',(-1.6865,1.07626632906913,0.739145673762293));
#17142=CARTESIAN_POINT('Ctrl Pts',(-1.6865,1.07057335460936,0.749669029712744));
#17143=CARTESIAN_POINT('Ctrl Pts',(-1.6865,1.04448849650432,0.797886398101832));
#17144=CARTESIAN_POINT('Ctrl Pts',(-1.6865,1.01542414332133,0.844202514930974));
#17145=CARTESIAN_POINT('Ctrl Pts',(-1.6865,0.98348603073344,0.888285135110482));
#17146=CARTESIAN_POINT('Ctrl Pts',(-1.6865,0.976132732681375,0.898434534020762));
#17147=CARTESIAN_POINT('Ctrl Pts',(-1.6865,0.968626883363404,0.908465522082479));
#17148=CARTESIAN_POINT('Ctrl Pts',(-1.6865,0.960969385665994,0.918373986113659));
#17149=CARTESIAN_POINT('Ctrl Pts',(-1.6865,0.928822249709468,0.959970961120058));
#17150=CARTESIAN_POINT('Ctrl Pts',(-1.6865,0.894006124211354,0.999410536617324));
#17151=CARTESIAN_POINT('Ctrl Pts',(-1.6865,0.856811235932228,1.03663507024378));
#17152=CARTESIAN_POINT('Ctrl Pts',(-1.6865,0.838875125773088,1.05458547597524));
#17153=CARTESIAN_POINT('Ctrl Pts',(-1.6865,0.820385172914883,1.07202043593171));
#17154=CARTESIAN_POINT('Ctrl Pts',(-1.6865,0.801370429731241,1.08893116790782));
#17155=CARTESIAN_POINT('Ctrl Pts',(-1.6865,0.789265686005685,1.09969650272226));
#17156=CARTESIAN_POINT('Ctrl Pts',(-1.6865,0.776948224556874,1.1102493585158));
#17157=CARTESIAN_POINT('Ctrl Pts',(-1.6865,0.764425135746565,1.12058710188661));
#17158=CARTESIAN_POINT('Ctrl Pts',(-1.6865,0.756948856335036,1.12675873087492));
#17159=CARTESIAN_POINT('Ctrl Pts',(-1.6865,0.749400063604347,1.13285292413839));
#17160=CARTESIAN_POINT('Ctrl Pts',(-1.6865,0.741790382865105,1.13886148265789));
#17161=CARTESIAN_POINT('Ctrl Pts',(-1.6865,0.698774277295606,1.17282674302192));
#17162=CARTESIAN_POINT('Ctrl Pts',(-1.6865,0.653734345483144,1.20412620058719));
#17163=CARTESIAN_POINT('Ctrl Pts',(-1.6865,0.607002895401327,1.23271172365974));
#17164=CARTESIAN_POINT('Ctrl Pts',(-1.6865,0.559252531102573,1.26192051427065));
#17165=CARTESIAN_POINT('Ctrl Pts',(-1.6865,0.50973534369957,1.28829637345923));
#17166=CARTESIAN_POINT('Ctrl Pts',(-1.6865,0.45876129133789,1.31175582276503));
#17167=CARTESIAN_POINT('Ctrl Pts',(-1.6865,0.430153328292115,1.32492187544713));
#17168=CARTESIAN_POINT('Ctrl Pts',(-1.6865,0.401085755513973,1.33716870507987));
#17169=CARTESIAN_POINT('Ctrl Pts',(-1.6865,0.37160881565879,1.34847609048941));
#17170=CARTESIAN_POINT('Ctrl Pts',(-1.6865,0.351783551682333,1.35608108278946));
#17171=CARTESIAN_POINT('Ctrl Pts',(-1.6865,0.331773048043608,1.36326103519375));
#17172=CARTESIAN_POINT('Ctrl Pts',(-1.6865,0.311591988507046,1.37000865843416));
#17173=CARTESIAN_POINT('Ctrl Pts',(-1.6865,0.296897647160957,1.37492177407063));
#17174=CARTESIAN_POINT('Ctrl Pts',(-1.6865,0.282106107519082,1.37960750309936));
#17175=CARTESIAN_POINT('Ctrl Pts',(-1.6865,0.267259363096465,1.38405235084035));
#17176=CARTESIAN_POINT('Ctrl Pts',(-1.6865,0.211486458549836,1.40074975343081));
#17177=CARTESIAN_POINT('Ctrl Pts',(-1.6865,0.154865348764943,1.41407827312293));
#17178=CARTESIAN_POINT('Ctrl Pts',(-1.6865,0.0977297285868856,1.42396068228593));
#17179=CARTESIAN_POINT('Ctrl Pts',(-1.6865,0.0383682737208729,1.43422808086617));
#17180=CARTESIAN_POINT('Ctrl Pts',(-1.6865,-0.0215495424099283,1.4407765896995));
#17181=CARTESIAN_POINT('Ctrl Pts',(-1.6865,-0.0816809005958121,1.44346955384022));
#17182=CARTESIAN_POINT('Ctrl Pts',(-1.6865,-0.138204235749947,1.44600093379366));
#17183=CARTESIAN_POINT('Ctrl Pts',(-1.6865,-0.194917405599328,1.44512562109251));
#17184=CARTESIAN_POINT('Ctrl Pts',(-1.6865,-0.25154665254263,1.44068090653038));
#17185=CARTESIAN_POINT('Ctrl Pts',(-1.6865,-0.255161436183491,1.44039718950508));
#17186=CARTESIAN_POINT('Ctrl Pts',(-1.6865,-0.258775878501556,1.44009891087668));
#17187=CARTESIAN_POINT('Ctrl Pts',(-1.6865,-0.26238990830909,1.43978602091337));
#17188=CARTESIAN_POINT('',(-1.6865,-1.4635,-1.79227059055215E-16));
#17189=CARTESIAN_POINT('Origin',(-1.6865,0.,0.));
#17190=CARTESIAN_POINT('',(-1.6865,-1.29040238558681,0.694864466152488));
#17191=CARTESIAN_POINT('Origin',(-1.6865,0.,0.));
#17192=CARTESIAN_POINT('Ctrl Pts',(-1.6865,-1.2904023855868,0.694864466152506));
#17193=CARTESIAN_POINT('Ctrl Pts',(-1.6865,-1.30885072776436,0.651973324418185));
#17194=CARTESIAN_POINT('Ctrl Pts',(-1.6865,-1.32508620682539,0.608247465432293));
#17195=CARTESIAN_POINT('Ctrl Pts',(-1.6865,-1.33896629703696,0.563783087832447));
#17196=CARTESIAN_POINT('Ctrl Pts',(-1.6865,-1.35596322182967,0.509334040996302));
#17197=CARTESIAN_POINT('Ctrl Pts',(-1.6865,-1.36942928069231,0.453776801997275));
#17198=CARTESIAN_POINT('Ctrl Pts',(-1.6865,-1.37942205624868,0.397441414603066));
#17199=CARTESIAN_POINT('Ctrl Pts',(-1.6865,-1.38232583274047,0.381071050568741));
#17200=CARTESIAN_POINT('Ctrl Pts',(-1.6865,-1.38493600923725,0.364635008432255));
#17201=CARTESIAN_POINT('Ctrl Pts',(-1.6865,-1.38725324896998,0.34814152080314));
#17202=CARTESIAN_POINT('Ctrl Pts',(-1.6865,-1.38960490215389,0.331403087507239));
#17203=CARTESIAN_POINT('Ctrl Pts',(-1.6865,-1.39165518732054,0.314600489882574));
#17204=CARTESIAN_POINT('Ctrl Pts',(-1.6865,-1.39340187668387,0.29777267933919));
#17205=CARTESIAN_POINT('Ctrl Pts',(-1.6865,-1.39934087814592,0.240555641485509));
#17206=CARTESIAN_POINT('Ctrl Pts',(-1.6865,-1.40178440679026,0.182987687587848));
#17207=CARTESIAN_POINT('Ctrl Pts',(-1.6865,-1.40079973123309,0.125409327587869));
#17208=CARTESIAN_POINT('Ctrl Pts',(-1.6865,-1.40013542640393,0.0865644691722947));
#17209=CARTESIAN_POINT('Ctrl Pts',(-1.6865,-1.39790967150014,0.047714876544446));
#17210=CARTESIAN_POINT('Ctrl Pts',(-1.6865,-1.39413032699431,0.00896907191044844));
#17211=CARTESIAN_POINT('Ctrl Pts',(-1.6865,-1.3924216166484,-0.00854861062335397));
#17212=CARTESIAN_POINT('Ctrl Pts',(-1.6865,-1.39039520209046,-0.0260450144637056));
#17213=CARTESIAN_POINT('Ctrl Pts',(-1.6865,-1.38805116691589,-0.0435097336037873));
#17214=CARTESIAN_POINT('Ctrl Pts',(-1.6865,-1.38659889452283,-0.0543301895998504));
#17215=CARTESIAN_POINT('Ctrl Pts',(-1.6865,-1.38502456181393,-0.0651386374936669));
#17216=CARTESIAN_POINT('Ctrl Pts',(-1.6865,-1.38333070427925,-0.075918112300396));
#17217=CARTESIAN_POINT('Ctrl Pts',(-1.6865,-1.3745984754921,-0.131488807173018));
#17218=CARTESIAN_POINT('Ctrl Pts',(-1.6865,-1.36268151203973,-0.186387190848527));
#17219=CARTESIAN_POINT('Ctrl Pts',(-1.6865,-1.34763859383464,-0.24029577530626));
#17220=CARTESIAN_POINT('Ctrl Pts',(-1.6865,-1.33296240556968,-0.292890127267258));
#17221=CARTESIAN_POINT('Ctrl Pts',(-1.6865,-1.31531029836967,-0.344543270611425));
#17222=CARTESIAN_POINT('Ctrl Pts',(-1.6865,-1.29469447197158,-0.39493657110514));
#17223=CARTESIAN_POINT('Ctrl Pts',(-1.6865,-1.28220200568538,-0.425473140210423));
#17224=CARTESIAN_POINT('Ctrl Pts',(-1.6865,-1.26862049403763,-0.455546579887635));
#17225=CARTESIAN_POINT('Ctrl Pts',(-1.6865,-1.25394594681483,-0.485079483421535));
#17226=CARTESIAN_POINT('Ctrl Pts',(-1.6865,-1.24672102839584,-0.499619817475368));
#17227=CARTESIAN_POINT('Ctrl Pts',(-1.6865,-1.2392310819698,-0.51402903840633));
#17228=CARTESIAN_POINT('Ctrl Pts',(-1.6865,-1.2314752167513,-0.528297362306323));
#17229=CARTESIAN_POINT('Ctrl Pts',(-1.6865,-1.2265591600616,-0.537341342208399));
#17230=CARTESIAN_POINT('Ctrl Pts',(-1.6865,-1.22153530521596,-0.546330365042694));
#17231=CARTESIAN_POINT('Ctrl Pts',(-1.6865,-1.216406396493,-0.555256606025037));
#17232=CARTESIAN_POINT('Ctrl Pts',(-1.6865,-1.19005780148628,-0.601113126637944));
#17233=CARTESIAN_POINT('Ctrl Pts',(-1.6865,-1.16104088129756,-0.645141987000547));
#17234=CARTESIAN_POINT('Ctrl Pts',(-1.6865,-1.12937946594324,-0.687054969399394));
#17235=CARTESIAN_POINT('Ctrl Pts',(-1.6865,-1.11768049850354,-0.702541914973292));
#17236=CARTESIAN_POINT('Ctrl Pts',(-1.6865,-1.1056200916295,-0.717739646605471));
#17237=CARTESIAN_POINT('Ctrl Pts',(-1.6865,-1.09319816065634,-0.732632329346327));
#17238=CARTESIAN_POINT('Ctrl Pts',(-1.6865,-1.05946030810074,-0.773080721432396));
#17239=CARTESIAN_POINT('Ctrl Pts',(-1.6865,-1.02305711561143,-0.811282018446671));
#17240=CARTESIAN_POINT('Ctrl Pts',(-1.6865,-0.984269503995115,-0.847108021494535));
#17241=CARTESIAN_POINT('Ctrl Pts',(-1.6865,-0.966400601050763,-0.863612553345551));
#17242=CARTESIAN_POINT('Ctrl Pts',(-1.6865,-0.948025344634025,-0.87961236447309));
#17243=CARTESIAN_POINT('Ctrl Pts',(-1.6865,-0.929170102459808,-0.895091662773315));
#17244=CARTESIAN_POINT('Ctrl Pts',(-1.6865,-0.915705894475452,-0.906145166612746));
#17245=CARTESIAN_POINT('Ctrl Pts',(-1.6865,-0.90199692206211,-0.916933210091794));
#17246=CARTESIAN_POINT('Ctrl Pts',(-1.6865,-0.888052703846498,-0.927449361680719));
#17247=CARTESIAN_POINT('Ctrl Pts',(-1.6865,-0.879943703448156,-0.933564833778548));
#17248=CARTESIAN_POINT('Ctrl Pts',(-1.6865,-0.871762069645838,-0.939583081642751));
#17249=CARTESIAN_POINT('Ctrl Pts',(-1.6865,-0.863513813439513,-0.945500676396998));
#17250=CARTESIAN_POINT('Ctrl Pts',(-1.6865,-0.820858663551776,-0.976103010381695));
#17251=CARTESIAN_POINT('Ctrl Pts',(-1.6865,-0.776391161968852,-1.00404189628927));
#17252=CARTESIAN_POINT('Ctrl Pts',(-1.6865,-0.730402963290917,-1.02921107378108));
#17253=CARTESIAN_POINT('Ctrl Pts',(-1.6865,-0.684629141529403,-1.05426292354938));
#17254=CARTESIAN_POINT('Ctrl Pts',(-1.6865,-0.637347598234742,-1.07657108217632));
#17255=CARTESIAN_POINT('Ctrl Pts',(-1.6865,-0.588833516322352,-1.09598122749975));
#17256=CARTESIAN_POINT('Ctrl Pts',(-1.6865,-0.564550715329474,-1.10569660657222));
#17257=CARTESIAN_POINT('Ctrl Pts',(-1.6865,-0.539959039562968,-1.1146851418401));
#17258=CARTESIAN_POINT('Ctrl Pts',(-1.6865,-0.515093195527775,-1.1229224840706));
#17259=CARTESIAN_POINT('Ctrl Pts',(-1.6865,-0.496768718082754,-1.12899285882626));
#17260=CARTESIAN_POINT('Ctrl Pts',(-1.6865,-0.478295351359644,-1.13465521308558));
#17261=CARTESIAN_POINT('Ctrl Pts',(-1.6865,-0.45968725369228,-1.13989858657083));
#17262=CARTESIAN_POINT('Ctrl Pts',(-1.6865,-0.450689443834044,-1.1424339815628));
#17263=CARTESIAN_POINT('Ctrl Pts',(-1.6865,-0.441661083642265,-1.14487103249921));
#17264=CARTESIAN_POINT('Ctrl Pts',(-1.6865,-0.432616279421598,-1.1472055526786));
#17265=CARTESIAN_POINT('Ctrl Pts',(-1.6865,-0.383781112234802,-1.15981021282161));
#17266=CARTESIAN_POINT('Ctrl Pts',(-1.6865,-0.334370220207706,-1.16945779617145));
#17267=CARTESIAN_POINT('Ctrl Pts',(-1.6865,-0.284637624516386,-1.17602215875609));
#17268=CARTESIAN_POINT('Ctrl Pts',(-1.6865,-0.235926324583538,-1.18245171728372));
#17269=CARTESIAN_POINT('Ctrl Pts',(-1.6865,-0.186905453024311,-1.18592341187249));
#17270=CARTESIAN_POINT('Ctrl Pts',(-1.6865,-0.137820117989715,-1.18626955672358));
#17271=CARTESIAN_POINT('Ctrl Pts',(-1.6865,-0.0887347829551201,-1.18661570157467));
#17272=CARTESIAN_POINT('Ctrl Pts',(-1.6865,-0.0395840767290218,-1.18383647660889));
#17273=CARTESIAN_POINT('Ctrl Pts',(-1.6865,0.00936663037056407,-1.17771275306651));
#17274=CARTESIAN_POINT('Ctrl Pts',(-7.90147783942094,-0.510216505388438,
1.06149619882937));
#17275=CARTESIAN_POINT('Ctrl Pts',(-7.87525430423351,-0.860016296466908,
0.89336217518757));
#17276=CARTESIAN_POINT('Ctrl Pts',(-7.82280723385865,-1.37476509314629,
0.187438301404127));
#17277=CARTESIAN_POINT('Ctrl Pts',(-7.74413662829635,-0.911603039763577,
-1.0476379059846));
#17278=CARTESIAN_POINT('Ctrl Pts',(-7.66546602273408,0.37338601803043,-1.33626108168095));
#17279=CARTESIAN_POINT('Ctrl Pts',(-7.58679541717176,1.32164391460705,-0.423509280609249));
#17280=CARTESIAN_POINT('Ctrl Pts',(-7.50812481160949,1.08034427095369,0.871377146278108));
#17281=CARTESIAN_POINT('Ctrl Pts',(-7.42945420604718,-0.133733706588163,
1.38132579741601));
#17282=CARTESIAN_POINT('Ctrl Pts',(-7.3507836004849,-1.22732977726997,0.647920010724189));
#17283=CARTESIAN_POINT('Ctrl Pts',(-7.27211299492261,-1.2160203437836,-0.668923549344045));
#17284=CARTESIAN_POINT('Ctrl Pts',(-7.19344238936034,-0.109920457047265,
-1.38347881456886));
#17285=CARTESIAN_POINT('Ctrl Pts',(-7.11477178379802,1.095127328248,-0.852540070304724));
#17286=CARTESIAN_POINT('Ctrl Pts',(-7.03610117823576,1.31425240912282,0.445947499710114));
#17287=CARTESIAN_POINT('Ctrl Pts',(-6.95743057267344,0.350169610287078,
1.34294482869753));
#17288=CARTESIAN_POINT('Ctrl Pts',(-6.87875996711116,-0.929164632477942,
1.03091115994185));
#17289=CARTESIAN_POINT('Ctrl Pts',(-6.80008936154887,-1.37198482640854,
-0.209241177774123));
#17290=CARTESIAN_POINT('Ctrl Pts',(-6.72141875598658,-0.579624239257938,
-1.26101500289363));
#17291=CARTESIAN_POINT('Ctrl Pts',(-6.64274815042429,0.734564342461029,
-1.17751395698303));
#17292=CARTESIAN_POINT('Ctrl Pts',(-6.564077544862,1.38743422631486,-0.0339118586638691));
#17293=CARTESIAN_POINT('Ctrl Pts',(-6.4854069392997,0.791214847056285,1.14022045088028));
#17294=CARTESIAN_POINT('Ctrl Pts',(-6.40673633373742,-0.517325047723218,
1.28782705533921));
#17295=CARTESIAN_POINT('Ctrl Pts',(-6.32806572817513,-1.36012387380599,
0.276019467196043));
#17296=CARTESIAN_POINT('Ctrl Pts',(-6.24939512261283,-0.978420656071388,
-0.984284868996692));
#17297=CARTESIAN_POINT('Ctrl Pts',(-6.17072451705056,0.284142091338451,
-1.35845020984985));
#17298=CARTESIAN_POINT('Ctrl Pts',(-6.09205391148824,1.29089537055166,-0.509620287250948));
#17299=CARTESIAN_POINT('Ctrl Pts',(-6.01338330592598,1.13547214593956,0.798014222500227));
#17300=CARTESIAN_POINT('Ctrl Pts',(-5.93471270036367,-0.0422020497217742,
1.38720679169256));
#17301=CARTESIAN_POINT('Ctrl Pts',(-5.85604209480139,-1.181882283109,0.727514923408978));
#17302=CARTESIAN_POINT('Ctrl Pts',(-5.77737148923909,-1.25752909475175,
-0.587149274616201));
#17303=CARTESIAN_POINT('Ctrl Pts',(-5.69870088367681,-0.201038633207167,
-1.37321053124158));
#17304=CARTESIAN_POINT('Ctrl Pts',(-5.62003027811452,1.03644432469548,-0.922988004686612));
#17305=CARTESIAN_POINT('Ctrl Pts',(-5.54135967255223,1.34082978479473,0.358188753595292));
#17306=CARTESIAN_POINT('Ctrl Pts',(-5.46268906698994,0.438083431536926,
1.31689278305031));
#17307=CARTESIAN_POINT('Ctrl Pts',(-5.38401846142764,-0.859063801779334,
1.09001517396937));
#17308=CARTESIAN_POINT('Ctrl Pts',(-5.30534785586536,-1.38280694114473,
-0.118189079598716));
#17309=CARTESIAN_POINT('Ctrl Pts',(-5.22667725030306,-0.66162677306598,
-1.21998922461717));
#17310=CARTESIAN_POINT('Ctrl Pts',(-5.14800664474078,0.655207470874117,
-1.22344875868442));
#17311=CARTESIAN_POINT('Ctrl Pts',(-5.06933603917847,1.38216685417029,-0.12545310777169));
#17312=CARTESIAN_POINT('Ctrl Pts',(-4.9906654336162,0.86477919209241,1.08548636285362));
#17313=CARTESIAN_POINT('Ctrl Pts',(-4.9119948280539,-0.431158056335988,
1.31917641938943));
#17314=CARTESIAN_POINT('Ctrl Pts',(-4.83332422249162,-1.33892925095376,
0.365228908983454));
#17315=CARTESIAN_POINT('Ctrl Pts',(-4.75465361692932,-1.04127965837587,
-0.917529491661948));
#17316=CARTESIAN_POINT('Ctrl Pts',(-4.67598301136704,0.193820620708426,
-1.37424788957624));
#17317=CARTESIAN_POINT('Ctrl Pts',(-4.59731240580474,1.25442668732974,-0.593748584109574));
#17318=CARTESIAN_POINT('Ctrl Pts',(-4.51864180024246,1.18568853815801,0.721294936553209));
#17319=CARTESIAN_POINT('Ctrl Pts',(-4.43997119468016,0.049490244982279,
1.38696590104707));
#17320=CARTESIAN_POINT('Ctrl Pts',(-4.36130058911787,-1.13126347935192,
0.803969299976234));
#17321=CARTESIAN_POINT('Ctrl Pts',(-4.28262998355558,-1.29355524026402,
-0.502830523536472));
#17322=CARTESIAN_POINT('Ctrl Pts',(-4.20395937799329,-0.29127585234018,
-1.35693849265711));
#17323=CARTESIAN_POINT('Ctrl Pts',(-4.125288772431,0.973235439907126,-0.989412185868934));
#17324=CARTESIAN_POINT('Ctrl Pts',(-4.04661816686871,1.36155538052876,0.268869188915402));
#17325=CARTESIAN_POINT('Ctrl Pts',(-3.96794756130642,0.524084520485498,
1.28509109030307));
#17326=CARTESIAN_POINT('Ctrl Pts',(-3.88927695574413,-0.785212894157578,
1.14436200828378));
#17327=CARTESIAN_POINT('Ctrl Pts',(-3.81060635018184,-1.38759323720175,
-0.0266214744418142));
#17328=CARTESIAN_POINT('Ctrl Pts',(-3.73193574461955,-0.740741232249389,
-1.17363798581818));
#17329=CARTESIAN_POINT('Ctrl Pts',(-3.65326513905726,0.572990579286003,
-1.26404331095425));
#17330=CARTESIAN_POINT('Ctrl Pts',(-3.57459453349497,1.3708663395606,-0.216446696849244));
#17331=CARTESIAN_POINT('Ctrl Pts',(-3.49592392793268,0.934568764120381,
1.02601409348018));
#17332=CARTESIAN_POINT('Ctrl Pts',(-3.41725332237039,-0.34310905511451,
1.34476759219195));
#17333=CARTESIAN_POINT('Ctrl Pts',(-3.3385827168081,-1.31189019805787,0.452844114240954));
#17334=CARTESIAN_POINT('Ctrl Pts',(-3.25991211124581,-1.09959347693818,
-0.846769085313812));
#17335=CARTESIAN_POINT('Ctrl Pts',(-3.18124150568352,0.102653133571944,
-1.38404698750922));
#17336=CARTESIAN_POINT('Ctrl Pts',(-3.10257090012123,1.2124824062959,-0.675285143647363));
#17337=CARTESIAN_POINT('Ctrl Pts',(-3.02390029455893,1.23072943933634,0.641427153820911));
#17338=CARTESIAN_POINT('Ctrl Pts',(-2.94522968899665,0.140966433426828,
1.38067098062933));
#17339=CARTESIAN_POINT('Ctrl Pts',(-2.86655908343435,-1.07570655288296,
0.876914196682235));
#17340=CARTESIAN_POINT('Ctrl Pts',(-2.78788847787207,-1.32393530813497,
-0.416316627394508));
#17341=CARTESIAN_POINT('Ctrl Pts',(-2.70921787230977,-0.38024109152726,
-1.33474396280885));
#17342=CARTESIAN_POINT('Ctrl Pts',(-2.63054726674748,0.905777314237609,
-1.05151653620214));
#17343=CARTESIAN_POINT('Ctrl Pts',(-2.5518766611852,1.37633981097026,0.178374023112081));
#17344=CARTESIAN_POINT('Ctrl Pts',(-2.4732060556229,0.607794121628612,1.24768375090184));
#17345=CARTESIAN_POINT('Ctrl Pts',(-2.39453545006062,-0.707927190944584,
1.19370650897096));
#17346=CARTESIAN_POINT('Ctrl Pts',(-2.31586484449832,-1.38633664878164,
0.0650760140720061));
#17347=CARTESIAN_POINT('Ctrl Pts',(-2.23719423893603,-0.81659578676643,
-1.12218984289901));
#17348=CARTESIAN_POINT('Ctrl Pts',(-2.15852363337374,0.488222034063068,
-1.29907078650092));
#17349=CARTESIAN_POINT('Ctrl Pts',(-2.07985302781145,1.35367817671458,-0.306589740084279));
#17350=CARTESIAN_POINT('Ctrl Pts',(-2.00118242224916,1.00009581383204,0.962242750523822));
#17351=CARTESIAN_POINT('Ctrl Pts',(-1.92251181668687,-0.253212907927416,
1.36414589400647));
#17352=CARTESIAN_POINT('Ctrl Pts',(-1.84384121112458,-1.2797987521583,0.539147881509388));
#17353=CARTESIAN_POINT('Ctrl Pts',(-1.76517060556229,-1.1517468612252,-0.773686852560318));
#17354=CARTESIAN_POINT('Ctrl Pts',(-1.71272353518743,-0.378730543625381,
-1.1807993824396));
#17355=CARTESIAN_POINT('Ctrl Pts',(-1.6865,0.00936663037056419,-1.17771275306651));
#17356=CARTESIAN_POINT('Ctrl Pts',(-7.84648522628062,-0.551480035117362,
1.14734422509853));
#17357=CARTESIAN_POINT('Ctrl Pts',(-7.82026169109319,-0.929569726514428,
0.965612438135244));
#17358=CARTESIAN_POINT('Ctrl Pts',(-7.76781462071833,-1.48594859993651,
0.202597289482033));
#17359=CARTESIAN_POINT('Ctrl Pts',(-7.68914401515604,-0.985328524405893,
-1.13236514907102));
#17360=CARTESIAN_POINT('Ctrl Pts',(-7.61047340959375,0.403583443814669,
-1.444330593912));
#17361=CARTESIAN_POINT('Ctrl Pts',(-7.53180280403146,1.42853127004439,-0.457760402645369));
#17362=CARTESIAN_POINT('Ctrl Pts',(-7.45313219846917,1.16771662655407,0.941849379929546));
#17363=CARTESIAN_POINT('Ctrl Pts',(-7.37446159290689,-0.144549359784947,
1.4930398982047));
#17364=CARTESIAN_POINT('Ctrl Pts',(-7.29579098734458,-1.32658951939263,
0.700320249332966));
#17365=CARTESIAN_POINT('Ctrl Pts',(-7.21712038178231,-1.31436544057442,
-0.72302243966458));
#17366=CARTESIAN_POINT('Ctrl Pts',(-7.13844977622001,-0.118810224428935,
-1.49536703964862));
#17367=CARTESIAN_POINT('Ctrl Pts',(-7.05977917065772,1.18369525693882,-0.921488863933704));
#17368=CARTESIAN_POINT('Ctrl Pts',(-6.98110856509543,1.42054197988822,0.482013302594748));
#17369=CARTESIAN_POINT('Ctrl Pts',(-6.90243795953314,0.378489419567362,
1.45155488595369));
#17370=CARTESIAN_POINT('Ctrl Pts',(-6.82376735397085,-1.00431040300948,
1.11428563498703));
#17371=CARTESIAN_POINT('Ctrl Pts',(-6.74509674840856,-1.48294348038045,
-0.22616346364377));
#17372=CARTESIAN_POINT('Ctrl Pts',(-6.66642614284627,-0.62650108815569,
-1.36299902244414));
#17373=CARTESIAN_POINT('Ctrl Pts',(-6.58775553728398,0.79397190231618,-1.27274486711051));
#17374=CARTESIAN_POINT('Ctrl Pts',(-6.50908493172169,1.49964234353539,-0.0366544649366292));
#17375=CARTESIAN_POINT('Ctrl Pts',(-6.4304143261594,0.855203990917139,1.23243526552375));
#17376=CARTESIAN_POINT('Ctrl Pts',(-6.35174372059711,-0.559163477607003,
1.3919794875371));
#17377=CARTESIAN_POINT('Ctrl Pts',(-6.27307311503482,-1.4701232785863,0.298342417100889));
#17378=CARTESIAN_POINT('Ctrl Pts',(-6.19440250947252,-1.05754998529305,
-1.06388846379349));
#17379=CARTESIAN_POINT('Ctrl Pts',(-6.11573190391024,0.30712195480691,-1.46831425781266));
#17380=CARTESIAN_POINT('Ctrl Pts',(-6.03706129834795,1.39529595135832,-0.550835598106954));
#17381=CARTESIAN_POINT('Ctrl Pts',(-5.95839069278566,1.22730294356278,0.862553262783086));
#17382=CARTESIAN_POINT('Ctrl Pts',(-5.87972008722336,-0.0456151214568538,
1.49939651524061));
#17383=CARTESIAN_POINT('Ctrl Pts',(-5.80104948166107,-1.27746647964148,
0.786352364678105));
#17384=CARTESIAN_POINT('Ctrl Pts',(-5.72237887609879,-1.35923119305369,
-0.634634707354204));
#17385=CARTESIAN_POINT('Ctrl Pts',(-5.64370827053649,-0.217297541984914,
-1.48426831353898));
#17386=CARTESIAN_POINT('Ctrl Pts',(-5.56503766497421,1.12026629194425,-0.99763424323164));
#17387=CARTESIAN_POINT('Ctrl Pts',(-5.48636705941191,1.44926878882929,0.3871571074734));
#17388=CARTESIAN_POINT('Ctrl Pts',(-5.40769645384962,0.473513231455331,
1.4233958928661));
#17389=CARTESIAN_POINT('Ctrl Pts',(-5.32902584828733,-0.928540199248638,
1.17816965948887));
#17390=CARTESIAN_POINT('Ctrl Pts',(-5.25035524272504,-1.49464082876438,
-0.127747568099473));
#17391=CARTESIAN_POINT('Ctrl Pts',(-5.17168463716275,-0.715135539896414,
-1.31865530285515));
#17392=CARTESIAN_POINT('Ctrl Pts',(-5.09301403160046,0.708197079535336,
-1.3223946251796));
#17393=CARTESIAN_POINT('Ctrl Pts',(-5.01434342603817,1.4939489750446,-0.135599071274354));
#17394=CARTESIAN_POINT('Ctrl Pts',(-4.93567282047588,0.934717819175246,
1.17327458281694));
#17395=CARTESIAN_POINT('Ctrl Pts',(-4.85700221491359,-0.466027769658844,
1.42586421726407));
#17396=CARTESIAN_POINT('Ctrl Pts',(-4.7783316093513,-1.4472145501712,0.39476663225298));
#17397=CARTESIAN_POINT('Ctrl Pts',(-4.69966100378902,-1.12549268105498,
-0.991734275428277));
#17398=CARTESIAN_POINT('Ctrl Pts',(-4.62099039822671,0.209495775981166,
-1.48538956776103));
#17399=CARTESIAN_POINT('Ctrl Pts',(-4.54231979266444,1.35587787983082,-0.641767733026107));
#17400=CARTESIAN_POINT('Ctrl Pts',(-4.46364918710213,1.28158056385069,0.779629339191021));
#17401=CARTESIAN_POINT('Ctrl Pts',(-4.38497858153985,0.0534927462215688,
1.49913614267282));
#17402=CARTESIAN_POINT('Ctrl Pts',(-4.30630797597756,-1.22275390296327,
0.868989954463811));
#17403=CARTESIAN_POINT('Ctrl Pts',(-4.22763737041526,-1.39817093683387,
-0.543496715314725));
#17404=CARTESIAN_POINT('Ctrl Pts',(-4.14896676485299,-0.314832655511832,
-1.46668028117384));
#17405=CARTESIAN_POINT('Ctrl Pts',(-4.07029615929068,1.05194541711039,-1.069430450105));
#17406=CARTESIAN_POINT('Ctrl Pts',(-3.9916255537284,1.47167055776957,0.290613863289574));
#17407=CARTESIAN_POINT('Ctrl Pts',(-3.91295494816611,0.566469619679939,
1.38902225256277));
#17408=CARTESIAN_POINT('Ctrl Pts',(-3.83428434260381,-0.848716632785046,
1.23691176951412));
#17409=CARTESIAN_POINT('Ctrl Pts',(-3.75561373704153,-1.49981421435604,
-0.0287744741790862));
#17410=CARTESIAN_POINT('Ctrl Pts',(-3.67694313147923,-0.800648345279968,
-1.26855542852604));
#17411=CARTESIAN_POINT('Ctrl Pts',(-3.59827252591695,0.619330933925767,
-1.36627224355318));
#17412=CARTESIAN_POINT('Ctrl Pts',(-3.51960192035466,1.4817345364132,-0.2339517258239));
#17413=CARTESIAN_POINT('Ctrl Pts',(-3.44093131479236,1.01015159136086,1.10899252048419));
#17414=CARTESIAN_POINT('Ctrl Pts',(-3.36226070923008,-0.370857845180013,
1.45352506462352));
#17415=CARTESIAN_POINT('Ctrl Pts',(-3.28359010366778,-1.41798872606892,
0.489467677714918));
#17416=CARTESIAN_POINT('Ctrl Pts',(-3.2049194981055,-1.18852260338978,-0.915251153134768));
#17417=CARTESIAN_POINT('Ctrl Pts',(-3.1262488925432,0.110955159445615,-1.49598116331925));
#17418=CARTESIAN_POINT('Ctrl Pts',(-3.04757828698092,1.31054137398826,-0.729898525037658));
#17419=CARTESIAN_POINT('Ctrl Pts',(-2.96890768141862,1.33026412759513,0.693302285556365));
#17420=CARTESIAN_POINT('Ctrl Pts',(-2.89023707585633,0.152367030144226,
1.49233212340576));
#17421=CARTESIAN_POINT('Ctrl Pts',(-2.81156647029404,-1.1627038351263,0.947834236787512));
#17422=CARTESIAN_POINT('Ctrl Pts',(-2.73289586473176,-1.43100797899029,
-0.449986046846273));
#17423=CARTESIAN_POINT('Ctrl Pts',(-2.65422525916946,-0.410992918288442,
-1.44269077873544));
#17424=CARTESIAN_POINT('Ctrl Pts',(-2.57555465360718,0.979031645955821,
-1.13655746175787));
#17425=CARTESIAN_POINT('Ctrl Pts',(-2.49688404804488,1.48765067235418,0.192799941771742));
#17426=CARTESIAN_POINT('Ctrl Pts',(-2.41821344248259,0.65694919705645,1.34858961146087));
#17427=CARTESIAN_POINT('Ctrl Pts',(-2.3395428369203,-0.765180483186115,
1.29024698443646));
#17428=CARTESIAN_POINT('Ctrl Pts',(-2.26087223135801,-1.49845599991427,
0.0703390073561241));
#17429=CARTESIAN_POINT('Ctrl Pts',(-2.18220162579572,-0.882637602677711,
-1.21294644025509));
#17430=CARTESIAN_POINT('Ctrl Pts',(-2.10353102023343,0.52770677084464,-1.40413255038478));
#17431=CARTESIAN_POINT('Ctrl Pts',(-2.02486041467114,1.4631562886501,-0.33138504701957));
#17432=CARTESIAN_POINT('Ctrl Pts',(-1.94618980910885,1.08097811166053,1.04006369893171));
#17433=CARTESIAN_POINT('Ctrl Pts',(-1.86751920354656,-0.273691387638793,
1.47447057785628));
#17434=CARTESIAN_POINT('Ctrl Pts',(-1.78884859798427,-1.38330189895777,
0.582751223231977));
#17435=CARTESIAN_POINT('Ctrl Pts',(-1.71017799242198,-1.24489386910607,
-0.836258427772682));
#17436=CARTESIAN_POINT('Ctrl Pts',(-1.65773092204712,-0.409360205506362,
-1.27629599986891));
#17437=CARTESIAN_POINT('Ctrl Pts',(-1.63150738685969,0.0101241523767517,
-1.27295974073757));
#17438=CARTESIAN_POINT('Ctrl Pts',(-7.79149261314031,-0.592743564846287,
1.23319225136769));
#17439=CARTESIAN_POINT('Ctrl Pts',(-7.76526907795288,-0.999123156561948,
1.03786270108292));
#17440=CARTESIAN_POINT('Ctrl Pts',(-7.71282200757802,-1.59713210672673,
0.21775627755994));
#17441=CARTESIAN_POINT('Ctrl Pts',(-7.63415140201573,-1.05905400904821,
-1.21709239215744));
#17442=CARTESIAN_POINT('Ctrl Pts',(-7.55548079645344,0.433780869598909,
-1.55240010614304));
#17443=CARTESIAN_POINT('Ctrl Pts',(-7.47681019089115,1.53541862548172,-0.492011524681491));
#17444=CARTESIAN_POINT('Ctrl Pts',(-7.39813958532886,1.25508898215445,1.01232161358098));
#17445=CARTESIAN_POINT('Ctrl Pts',(-7.31946897976657,-0.155365012981731,
1.60475399899339));
#17446=CARTESIAN_POINT('Ctrl Pts',(-7.24079837420427,-1.42584926151528,
0.752720487941745));
#17447=CARTESIAN_POINT('Ctrl Pts',(-7.16212776864199,-1.41271053736525,
-0.777121329985117));
#17448=CARTESIAN_POINT('Ctrl Pts',(-7.08345716307969,-0.127699991810606,
-1.60725526472837));
#17449=CARTESIAN_POINT('Ctrl Pts',(-7.00478655751741,1.27226318562964,-0.990437657562687));
#17450=CARTESIAN_POINT('Ctrl Pts',(-6.92611595195512,1.52683155065362,0.518079105479383));
#17451=CARTESIAN_POINT('Ctrl Pts',(-6.84744534639283,0.406809228847646,
1.56016494320984));
#17452=CARTESIAN_POINT('Ctrl Pts',(-6.76877474083054,-1.07945617354101,
1.19766011003222));
#17453=CARTESIAN_POINT('Ctrl Pts',(-6.69010413526824,-1.59390213435235,
-0.243085749513416));
#17454=CARTESIAN_POINT('Ctrl Pts',(-6.61143352970597,-0.673377937053443,
-1.46498304199465));
#17455=CARTESIAN_POINT('Ctrl Pts',(-6.53276292414366,0.853379462171331,
-1.36797577723799));
#17456=CARTESIAN_POINT('Ctrl Pts',(-6.45409231858138,1.61185046075593,-0.0393970712093886));
#17457=CARTESIAN_POINT('Ctrl Pts',(-6.37542171301908,0.919193134777992,
1.32465008016721));
#17458=CARTESIAN_POINT('Ctrl Pts',(-6.2967511074568,-0.601001907490788,
1.49613191973499));
#17459=CARTESIAN_POINT('Ctrl Pts',(-6.2180805018945,-1.58012268336662,0.320665367005734));
#17460=CARTESIAN_POINT('Ctrl Pts',(-6.13940989633221,-1.1366793145147,-1.14349205859028));
#17461=CARTESIAN_POINT('Ctrl Pts',(-6.06073929076993,0.330101818275368,
-1.57817830577548));
#17462=CARTESIAN_POINT('Ctrl Pts',(-5.98206868520763,1.49969653216498,-0.592050908962961));
#17463=CARTESIAN_POINT('Ctrl Pts',(-5.90339807964535,1.319133741186,0.927092303065946));
#17464=CARTESIAN_POINT('Ctrl Pts',(-5.82472747408305,-0.0490281931919314,
1.61158623878866));
#17465=CARTESIAN_POINT('Ctrl Pts',(-5.74605686852077,-1.37305067617395,
0.845189805947231));
#17466=CARTESIAN_POINT('Ctrl Pts',(-5.66738626295846,-1.46093329135563,
-0.682120140092207));
#17467=CARTESIAN_POINT('Ctrl Pts',(-5.5887156573962,-0.233556450762664,
-1.59532609583638));
#17468=CARTESIAN_POINT('Ctrl Pts',(-5.51004505183388,1.20408825919302,-1.07228048177667));
#17469=CARTESIAN_POINT('Ctrl Pts',(-5.43137444627161,1.55770779286385,0.416125461351507));
#17470=CARTESIAN_POINT('Ctrl Pts',(-5.35270384070931,0.508943031373735,
1.52989900268188));
#17471=CARTESIAN_POINT('Ctrl Pts',(-5.27403323514702,-0.998016596717941,
1.26632414500837));
#17472=CARTESIAN_POINT('Ctrl Pts',(-5.19536262958473,-1.60647471638402,
-0.13730605660023));
#17473=CARTESIAN_POINT('Ctrl Pts',(-5.11669202402244,-0.768644306726847,
-1.41732138109313));
#17474=CARTESIAN_POINT('Ctrl Pts',(-5.03802141846015,0.761186688196555,
-1.42134049167478));
#17475=CARTESIAN_POINT('Ctrl Pts',(-4.95935081289786,1.60573109591891,-0.145745034777019));
#17476=CARTESIAN_POINT('Ctrl Pts',(-4.88068020733557,1.00465644625808,1.26106280278026));
#17477=CARTESIAN_POINT('Ctrl Pts',(-4.80200960177328,-0.5008974829817,1.5325520151387));
#17478=CARTESIAN_POINT('Ctrl Pts',(-4.72333899621098,-1.55549984938864,
0.424304355522506));
#17479=CARTESIAN_POINT('Ctrl Pts',(-4.6446683906487,-1.20970570373407,-1.0659390591946));
#17480=CARTESIAN_POINT('Ctrl Pts',(-4.5659977850864,0.225170931253902,-1.59653124594583));
#17481=CARTESIAN_POINT('Ctrl Pts',(-4.48732717952412,1.45732907233191,-0.689786881942641));
#17482=CARTESIAN_POINT('Ctrl Pts',(-4.40865657396183,1.37747258954337,0.837963741828835));
#17483=CARTESIAN_POINT('Ctrl Pts',(-4.32998596839954,0.0574952474608585,
1.61130638429858));
#17484=CARTESIAN_POINT('Ctrl Pts',(-4.25131536283725,-1.31424432657462,
0.93401060895139));
#17485=CARTESIAN_POINT('Ctrl Pts',(-4.17264475727496,-1.50278663340373,
-0.584162907092979));
#17486=CARTESIAN_POINT('Ctrl Pts',(-4.09397415171267,-0.338389458683483,
-1.57642206969058));
#17487=CARTESIAN_POINT('Ctrl Pts',(-4.01530354615038,1.13065539431366,-1.14944871434106));
#17488=CARTESIAN_POINT('Ctrl Pts',(-3.93663294058808,1.58178573501038,0.312358537663747));
#17489=CARTESIAN_POINT('Ctrl Pts',(-3.85796233502579,0.608854718874381,
1.49295341482247));
#17490=CARTESIAN_POINT('Ctrl Pts',(-3.77929172946351,-0.912220371412514,
1.32946153074446));
#17491=CARTESIAN_POINT('Ctrl Pts',(-3.70062112390121,-1.61203519151034,
-0.0309274739163594));
#17492=CARTESIAN_POINT('Ctrl Pts',(-3.62195051833893,-0.860555458310546,
-1.36347287123389));
#17493=CARTESIAN_POINT('Ctrl Pts',(-3.54327991277663,0.665671288565531,
-1.46850117615212));
#17494=CARTESIAN_POINT('Ctrl Pts',(-3.46460930721435,1.59260273326579,-0.251456754798555));
#17495=CARTESIAN_POINT('Ctrl Pts',(-3.38593870165205,1.08573441860134,1.19197094748821));
#17496=CARTESIAN_POINT('Ctrl Pts',(-3.30726809608977,-0.398606635245517,
1.56228253705509));
#17497=CARTESIAN_POINT('Ctrl Pts',(-3.22859749052747,-1.52408725407996,
0.526091241188881));
#17498=CARTESIAN_POINT('Ctrl Pts',(-3.14992688496519,-1.27745172984138,
-0.983733220955725));
#17499=CARTESIAN_POINT('Ctrl Pts',(-3.07125627940289,0.119257185319287,
-1.60791533912927));
#17500=CARTESIAN_POINT('Ctrl Pts',(-2.99258567384061,1.40860034168063,-0.784511906427953));
#17501=CARTESIAN_POINT('Ctrl Pts',(-2.9139150682783,1.42979881585392,0.745177417291821));
#17502=CARTESIAN_POINT('Ctrl Pts',(-2.83524446271603,0.163767626861624,
1.60399326618219));
#17503=CARTESIAN_POINT('Ctrl Pts',(-2.75657385715372,-1.24970111736964,
1.01875427689279));
#17504=CARTESIAN_POINT('Ctrl Pts',(-2.67790325159145,-1.53808064984562,
-0.48365546629804));
#17505=CARTESIAN_POINT('Ctrl Pts',(-2.59923264602914,-0.441744745049623,
-1.55063759466203));
#17506=CARTESIAN_POINT('Ctrl Pts',(-2.52056204046686,1.05228597767403,-1.2215983873136));
#17507=CARTESIAN_POINT('Ctrl Pts',(-2.44189143490457,1.59896153373811,0.207225860431403));
#17508=CARTESIAN_POINT('Ctrl Pts',(-2.36322082934228,0.706104272484286,
1.4494954720199));
#17509=CARTESIAN_POINT('Ctrl Pts',(-2.28455022377999,-0.822433775427645,
1.38678745990196));
#17510=CARTESIAN_POINT('Ctrl Pts',(-2.2058796182177,-1.6105753510469,0.0756020006402417));
#17511=CARTESIAN_POINT('Ctrl Pts',(-2.12720901265541,-0.948679418588992,
-1.30370303761117));
#17512=CARTESIAN_POINT('Ctrl Pts',(-2.04853840709312,0.567191507626213,
-1.50919431426864));
#17513=CARTESIAN_POINT('Ctrl Pts',(-1.96986780153083,1.57263440058562,-0.35618035395486));
#17514=CARTESIAN_POINT('Ctrl Pts',(-1.89119719596854,1.16186040948903,1.11788464733959));
#17515=CARTESIAN_POINT('Ctrl Pts',(-1.81252659040625,-0.294169867350172,
1.58479526170609));
#17516=CARTESIAN_POINT('Ctrl Pts',(-1.73385598484396,-1.48680504575724,
0.626354564954566));
#17517=CARTESIAN_POINT('Ctrl Pts',(-1.65518537928167,-1.33804087698695,
-0.898830002985046));
#17518=CARTESIAN_POINT('Ctrl Pts',(-1.60273830890681,-0.439989867387345,
-1.37179261729822));
#17519=CARTESIAN_POINT('Ctrl Pts',(-1.57651477371938,0.0108816743829391,
-1.36820672840862));
#17520=CARTESIAN_POINT('Ctrl Pts',(-7.7365,-0.634007094575211,1.31904027763685));
#17521=CARTESIAN_POINT('Ctrl Pts',(-7.71027646481257,-1.06867658660947,
1.11011296403059));
#17522=CARTESIAN_POINT('Ctrl Pts',(-7.65782939443771,-1.70831561351695,
0.232915265637844));
#17523=CARTESIAN_POINT('Ctrl Pts',(-7.57915878887542,-1.13277949369053,
-1.30181963524385));
#17524=CARTESIAN_POINT('Ctrl Pts',(-7.50048818331312,0.463978295383148,
-1.66046961837409));
#17525=CARTESIAN_POINT('Ctrl Pts',(-7.42181757775084,1.64230598091905,-0.526262646717611));
#17526=CARTESIAN_POINT('Ctrl Pts',(-7.34314697218855,1.34246133775483,1.08279384723242));
#17527=CARTESIAN_POINT('Ctrl Pts',(-7.26447636662625,-0.166180666178515,
1.71646809978208));
#17528=CARTESIAN_POINT('Ctrl Pts',(-7.18580576106397,-1.52510900363794,
0.805120726550522));
#17529=CARTESIAN_POINT('Ctrl Pts',(-7.10713515550167,-1.51105563415607,
-0.831220220305652));
#17530=CARTESIAN_POINT('Ctrl Pts',(-7.0284645499394,-0.136589759192276,
-1.71914348980813));
#17531=CARTESIAN_POINT('Ctrl Pts',(-6.94979394437708,1.36083111432046,-1.05938645119167));
#17532=CARTESIAN_POINT('Ctrl Pts',(-6.87112333881482,1.63312112141902,0.554144908364018));
#17533=CARTESIAN_POINT('Ctrl Pts',(-6.7924527332525,0.43512903812793,1.668775000466));
#17534=CARTESIAN_POINT('Ctrl Pts',(-6.71378212769024,-1.15460194407255,
1.28103458507741));
#17535=CARTESIAN_POINT('Ctrl Pts',(-6.63511152212792,-1.70486078832426,
-0.260008035383061));
#17536=CARTESIAN_POINT('Ctrl Pts',(-6.55644091656565,-0.720254785951196,
-1.56696706154517));
#17537=CARTESIAN_POINT('Ctrl Pts',(-6.47777031100335,0.912787022026482,
-1.46320668736547));
#17538=CARTESIAN_POINT('Ctrl Pts',(-6.39909970544107,1.72405857797647,-0.0421396774821499));
#17539=CARTESIAN_POINT('Ctrl Pts',(-6.32042909987877,0.983182278638845,
1.41686489481067));
#17540=CARTESIAN_POINT('Ctrl Pts',(-6.24175849431648,-0.642840337374572,
1.60028435193288));
#17541=CARTESIAN_POINT('Ctrl Pts',(-6.1630878887542,-1.69012208814694,0.342988316910582));
#17542=CARTESIAN_POINT('Ctrl Pts',(-6.08441728319189,-1.21580864373636,
-1.22309565338708));
#17543=CARTESIAN_POINT('Ctrl Pts',(-6.00574667762962,0.353081681743826,
-1.68804235373829));
#17544=CARTESIAN_POINT('Ctrl Pts',(-5.92707607206732,1.60409711297163,-0.633266219818969));
#17545=CARTESIAN_POINT('Ctrl Pts',(-5.84840546650504,1.41096453880922,0.991631343348807));
#17546=CARTESIAN_POINT('Ctrl Pts',(-5.76973486094274,-0.0524412649270098,
1.72377596233671));
#17547=CARTESIAN_POINT('Ctrl Pts',(-5.69106425538045,-1.46863487270643,
0.90402724721636));
#17548=CARTESIAN_POINT('Ctrl Pts',(-5.61239364981816,-1.56263538965757,
-0.729605572830212));
#17549=CARTESIAN_POINT('Ctrl Pts',(-5.53372304425587,-0.249815359540411,
-1.70638387813377));
#17550=CARTESIAN_POINT('Ctrl Pts',(-5.45505243869358,1.28791022644179,-1.1469267203217));
#17551=CARTESIAN_POINT('Ctrl Pts',(-5.37638183313129,1.66614679689841,0.445093815229617));
#17552=CARTESIAN_POINT('Ctrl Pts',(-5.297711227569,0.544372831292141,1.63640211249766));
#17553=CARTESIAN_POINT('Ctrl Pts',(-5.21904062200671,-1.06749299418725,
1.35447863052787));
#17554=CARTESIAN_POINT('Ctrl Pts',(-5.14037001644442,-1.71830860400367,
-0.14686454510099));
#17555=CARTESIAN_POINT('Ctrl Pts',(-5.06169941088213,-0.822153073557281,
-1.51598745933111));
#17556=CARTESIAN_POINT('Ctrl Pts',(-4.98302880531984,0.814176296857773,
-1.52028635816996));
#17557=CARTESIAN_POINT('Ctrl Pts',(-4.90435819975755,1.71751321679322,-0.155890998279683));
#17558=CARTESIAN_POINT('Ctrl Pts',(-4.82568759419526,1.07459507334092,1.34885102274358));
#17559=CARTESIAN_POINT('Ctrl Pts',(-4.74701698863297,-0.535767196304556,
1.63923981301333));
#17560=CARTESIAN_POINT('Ctrl Pts',(-4.66834638307067,-1.66378514860608,
0.453842078792031));
#17561=CARTESIAN_POINT('Ctrl Pts',(-4.58967577750839,-1.29391872641317,
-1.14014384296093));
#17562=CARTESIAN_POINT('Ctrl Pts',(-4.51100517194609,0.240846086526641,
-1.70767292413062));
#17563=CARTESIAN_POINT('Ctrl Pts',(-4.43233456638381,1.55878026483299,-0.737806030859172));
#17564=CARTESIAN_POINT('Ctrl Pts',(-4.35366396082151,1.47336461523605,0.896298144466647));
#17565=CARTESIAN_POINT('Ctrl Pts',(-4.27499335525922,0.0614977487001475,
1.72347662592433));
#17566=CARTESIAN_POINT('Ctrl Pts',(-4.19632274969694,-1.40573475018597,
0.999031263438967));
#17567=CARTESIAN_POINT('Ctrl Pts',(-4.11765214413464,-1.60740232997359,
-0.624829098871234));
#17568=CARTESIAN_POINT('Ctrl Pts',(-4.03898153857236,-0.361946261855135,
-1.68616385820732));
#17569=CARTESIAN_POINT('Ctrl Pts',(-3.96031093301006,1.20936537151692,-1.22946697857712));
#17570=CARTESIAN_POINT('Ctrl Pts',(-3.88164032744778,1.69190091225119,0.334103212037918));
#17571=CARTESIAN_POINT('Ctrl Pts',(-3.80296972188548,0.651239818068822,
1.59688457708217));
#17572=CARTESIAN_POINT('Ctrl Pts',(-3.72429911632319,-0.975724110039982,
1.4220112919748));
#17573=CARTESIAN_POINT('Ctrl Pts',(-3.6456285107609,-1.72425616866463,-0.0330804736536309));
#17574=CARTESIAN_POINT('Ctrl Pts',(-3.56695790519861,-0.920462571341124,
-1.45839031394175));
#17575=CARTESIAN_POINT('Ctrl Pts',(-3.48828729963632,0.712011643205295,
-1.57073010875106));
#17576=CARTESIAN_POINT('Ctrl Pts',(-3.40961669407403,1.70347093011839,-0.26896178377321));
#17577=CARTESIAN_POINT('Ctrl Pts',(-3.33094608851174,1.16131724584182,1.27494937449222));
#17578=CARTESIAN_POINT('Ctrl Pts',(-3.25227548294945,-0.426355425311021,
1.67104000948667));
#17579=CARTESIAN_POINT('Ctrl Pts',(-3.17360487738716,-1.63018578209101,
0.562714804662844));
#17580=CARTESIAN_POINT('Ctrl Pts',(-3.09493427182487,-1.36638085629297,
-1.05221528877668));
#17581=CARTESIAN_POINT('Ctrl Pts',(-3.01626366626258,0.12755921119296,-1.71984951493929));
#17582=CARTESIAN_POINT('Ctrl Pts',(-2.93759306070029,1.50665930937299,-0.839125287818249));
#17583=CARTESIAN_POINT('Ctrl Pts',(-2.858922455138,1.52933350411271,0.797052549027277));
#17584=CARTESIAN_POINT('Ctrl Pts',(-2.78025184957571,0.175168223579021,
1.71565440895862));
#17585=CARTESIAN_POINT('Ctrl Pts',(-2.70158124401342,-1.33669839961298,
1.08967431699807));
#17586=CARTESIAN_POINT('Ctrl Pts',(-2.62291063845113,-1.64515332070094,
-0.517324885749805));
#17587=CARTESIAN_POINT('Ctrl Pts',(-2.54424003288884,-0.472496571810804,
-1.65858441058862));
#17588=CARTESIAN_POINT('Ctrl Pts',(-2.46556942732655,1.12554030939224,-1.30663931286933));
#17589=CARTESIAN_POINT('Ctrl Pts',(-2.38689882176426,1.71027239512204,0.221651779091063));
#17590=CARTESIAN_POINT('Ctrl Pts',(-2.30822821620197,0.755259347912122,
1.55040133257893));
#17591=CARTESIAN_POINT('Ctrl Pts',(-2.22955761063968,-0.879687067669174,
1.48332793536745));
#17592=CARTESIAN_POINT('Ctrl Pts',(-2.15088700507738,-1.72269470217952,
0.0808649939243594));
#17593=CARTESIAN_POINT('Ctrl Pts',(-2.0722163995151,-1.01472123450027,-1.39445963496725));
#17594=CARTESIAN_POINT('Ctrl Pts',(-1.9935457939528,0.606676244407784,-1.6142560781525));
#17595=CARTESIAN_POINT('Ctrl Pts',(-1.91487518839052,1.68211251252115,-0.380975660890149));
#17596=CARTESIAN_POINT('Ctrl Pts',(-1.83620458282822,1.24274270731752,1.19570559574748));
#17597=CARTESIAN_POINT('Ctrl Pts',(-1.75753397726594,-0.314648347061551,
1.6951199455559));
#17598=CARTESIAN_POINT('Ctrl Pts',(-1.67886337170364,-1.5903081925567,0.669957906677155));
#17599=CARTESIAN_POINT('Ctrl Pts',(-1.60019276614136,-1.43118788486783,
-0.96140157819741));
#17600=CARTESIAN_POINT('Ctrl Pts',(-1.54774569576649,-0.470619529268327,
-1.46728923472753));
#17601=CARTESIAN_POINT('Ctrl Pts',(-1.52152216057906,0.0116391963891266,
-1.46345371607968));
#17602=CARTESIAN_POINT('Ctrl Pts',(-2.14715504584291,-1.46566693596749,
0.000405098676182412));
#17603=CARTESIAN_POINT('Ctrl Pts',(-2.12217549706697,-1.46397116480163,
-0.45709640867042));
#17604=CARTESIAN_POINT('Ctrl Pts',(-2.09719594829103,-1.23229569088932,
-0.91608689002793));
#17605=CARTESIAN_POINT('Ctrl Pts',(-2.0722163995151,-0.862483899295466,
-1.18520493734953));
#17606=CARTESIAN_POINT('Ctrl Pts',(-2.04599286432767,-0.474255408197588,
-1.467725116029));
#17607=CARTESIAN_POINT('Ctrl Pts',(-2.01976932914024,0.0662104181050797,
-1.54099059709075));
#17608=CARTESIAN_POINT('Ctrl Pts',(-1.99354579395281,0.51568270927531,-1.37207660141124));
#17609=CARTESIAN_POINT('Ctrl Pts',(-1.96732225876538,0.965155000445553,
-1.20316260573173));
#17610=CARTESIAN_POINT('Ctrl Pts',(-1.94109872357795,1.32363375648335,-0.792069133310953));
#17611=CARTESIAN_POINT('Ctrl Pts',(-1.91487518839052,1.42964483363498,-0.323742187660957));
#17612=CARTESIAN_POINT('Ctrl Pts',(-1.88865165320309,1.53565591078661,0.14458475798904));
#17613=CARTESIAN_POINT('Ctrl Pts',(-1.86242811801566,1.38919930905206,0.670145176868271));
#17614=CARTESIAN_POINT('Ctrl Pts',(-1.83620458282822,1.05640583245494,1.01616111127595));
#17615=CARTESIAN_POINT('Ctrl Pts',(-1.8099810476408,0.723612355857827,1.36217704568362));
#17616=CARTESIAN_POINT('Ctrl Pts',(-1.78375751245337,0.204482004398144,
1.52864849561976));
#17617=CARTESIAN_POINT('Ctrl Pts',(-1.75753397726594,-0.267693145580892,
1.44102388077471));
#17618=CARTESIAN_POINT('Ctrl Pts',(-1.73385598484396,-0.694033817925085,
1.3619050681718));
#17619=CARTESIAN_POINT('Ctrl Pts',(-1.71017799242198,-1.0820928104985,1.07562658259897));
#17620=CARTESIAN_POINT('Ctrl Pts',(-1.6865,-1.29040238558681,0.694864466152488));
#17621=CARTESIAN_POINT('',(-7.7365,-0.684664424539443,-0.95829519891841));
#17622=CARTESIAN_POINT('Ctrl Pts',(-7.7365,-0.686089228034751,-0.959351223124451));
#17623=CARTESIAN_POINT('Ctrl Pts',(-7.7365,-0.719567521781266,-0.941182198525624));
#17624=CARTESIAN_POINT('Ctrl Pts',(-7.7365,-0.752028806414924,-0.921351335407023));
#17625=CARTESIAN_POINT('Ctrl Pts',(-7.7365,-0.783331577414887,-0.899889939916658));
#17626=CARTESIAN_POINT('Ctrl Pts',(-7.7365,-0.823255286032892,-0.872517970192505));
#17627=CARTESIAN_POINT('Ctrl Pts',(-7.7365,-0.861295942401313,-0.842495516275831));
#17628=CARTESIAN_POINT('Ctrl Pts',(-7.7365,-0.897382909658782,-0.810117125580153));
#17629=CARTESIAN_POINT('Ctrl Pts',(-7.7365,-0.910704143482914,-0.798164885032232));
#17630=CARTESIAN_POINT('Ctrl Pts',(-7.7365,-0.923758957569899,-0.785891136787456));
#17631=CARTESIAN_POINT('Ctrl Pts',(-7.7365,-0.93654302005363,-0.773309146568843));
#17632=CARTESIAN_POINT('Ctrl Pts',(-7.7365,-0.944204342863284,-0.765768923046361));
#17633=CARTESIAN_POINT('Ctrl Pts',(-7.7365,-0.951765482935571,-0.75812076753032));
#17634=CARTESIAN_POINT('Ctrl Pts',(-7.7365,-0.959220174508566,-0.750373653173739));
#17635=CARTESIAN_POINT('Ctrl Pts',(-7.7365,-0.994284459823726,-0.713933912440213));
#17636=CARTESIAN_POINT('Ctrl Pts',(-7.7365,-1.02703314687708,-0.675271898636465));
#17637=CARTESIAN_POINT('Ctrl Pts',(-7.7365,-1.05739069023667,-0.634712603653476));
#17638=CARTESIAN_POINT('Ctrl Pts',(-7.7365,-1.07909989922968,-0.605707944054868));
#17639=CARTESIAN_POINT('Ctrl Pts',(-7.7365,-1.09958591366534,-0.575731842990991));
#17640=CARTESIAN_POINT('Ctrl Pts',(-7.7365,-1.11881249318271,-0.54488942520468));
#17641=CARTESIAN_POINT('Ctrl Pts',(-7.7365,-1.12494218476806,-0.535056448485871));
#17642=CARTESIAN_POINT('Ctrl Pts',(-7.7365,-1.13094380182462,-0.525135342523029));
#17643=CARTESIAN_POINT('Ctrl Pts',(-7.7365,-1.13681598362796,-0.515129316344604));
#17644=CARTESIAN_POINT('Ctrl Pts',(-7.7365,-1.14155088186925,-0.507061188118799));
#17645=CARTESIAN_POINT('Ctrl Pts',(-7.7365,-1.14620080441806,-0.498939107641481));
#17646=CARTESIAN_POINT('Ctrl Pts',(-7.7365,-1.15076055599585,-0.490773281325137));
#17647=CARTESIAN_POINT('Ctrl Pts',(-7.7365,-1.17633138736302,-0.444979784871117));
#17648=CARTESIAN_POINT('Ctrl Pts',(-7.7365,-1.19911090769331,-0.397742968678235));
#17649=CARTESIAN_POINT('Ctrl Pts',(-7.7365,-1.2190202952071,-0.349393168832874));
#17650=CARTESIAN_POINT('Ctrl Pts',(-7.7365,-1.2393257464617,-0.30008153113184));
#17651=CARTESIAN_POINT('Ctrl Pts',(-7.7365,-1.25664650233717,-0.249611304674763));
#17652=CARTESIAN_POINT('Ctrl Pts',(-7.7365,-1.27086282858701,-0.198293772224332));
#17653=CARTESIAN_POINT('Ctrl Pts',(-7.7365,-1.27935267763108,-0.167647450793473));
#17654=CARTESIAN_POINT('Ctrl Pts',(-7.7365,-1.2867346336525,-0.136698263002545));
#17655=CARTESIAN_POINT('Ctrl Pts',(-7.7365,-1.29297548212098,-0.105508124729707));
#17656=CARTESIAN_POINT('Ctrl Pts',(-7.7365,-1.29611179238721,-0.0898336613351524));
#17657=CARTESIAN_POINT('Ctrl Pts',(-7.7365,-1.29895981553652,-0.0740983053561009));
#17658=CARTESIAN_POINT('Ctrl Pts',(-7.7365,-1.30151470570495,-0.0583097264166406));
#17659=CARTESIAN_POINT('Ctrl Pts',(-7.7365,-1.30342781450681,-0.0464871949783093));
#17660=CARTESIAN_POINT('Ctrl Pts',(-7.7365,-1.30517672269469,-0.0346323680336482));
#17661=CARTESIAN_POINT('Ctrl Pts',(-7.7365,-1.3067565281468,-0.0227722525703492));
#17662=CARTESIAN_POINT('Ctrl Pts',(-7.7365,-1.31399492195315,0.0315687336550901));
#17663=CARTESIAN_POINT('Ctrl Pts',(-7.7365,-1.31770532384574,0.086122873391717));
#17664=CARTESIAN_POINT('Ctrl Pts',(-7.7365,-1.31777798642413,0.140559222914643));
#17665=CARTESIAN_POINT('Ctrl Pts',(-7.7365,-1.31779471615732,0.153092573965366));
#17666=CARTESIAN_POINT('Ctrl Pts',(-7.7365,-1.31761842432871,0.165619795498501));
#17667=CARTESIAN_POINT('Ctrl Pts',(-7.7365,-1.31724742365147,0.178137029012559));
#17668=CARTESIAN_POINT('Ctrl Pts',(-7.7365,-1.31568993550475,0.230685296506085));
#17669=CARTESIAN_POINT('Ctrl Pts',(-7.7365,-1.31070510000365,0.283056976251484));
#17670=CARTESIAN_POINT('Ctrl Pts',(-7.7365,-1.3024938347724,0.335034845453329));
#17671=CARTESIAN_POINT('Ctrl Pts',(-7.7365,-1.29853419969743,0.360099605659894));
#17672=CARTESIAN_POINT('Ctrl Pts',(-7.7365,-1.293823524476,0.385072900683143));
#17673=CARTESIAN_POINT('Ctrl Pts',(-7.7365,-1.28838015099446,0.409930549200139));
#17674=CARTESIAN_POINT('Ctrl Pts',(-7.7365,-1.28491491105284,0.425754875197221));
#17675=CARTESIAN_POINT('Ctrl Pts',(-7.7365,-1.28115268656436,0.441532333910416));
#17676=CARTESIAN_POINT('Ctrl Pts',(-7.7365,-1.27709766589713,0.457256627308522));
#17677=CARTESIAN_POINT('Ctrl Pts',(-7.7365,-1.27467681968889,0.466644026084986));
#17678=CARTESIAN_POINT('Ctrl Pts',(-7.7365,-1.27215179327647,0.476011400153136));
#17679=CARTESIAN_POINT('Ctrl Pts',(-7.7365,-1.26952717248285,0.485345283174778));
#17680=CARTESIAN_POINT('Ctrl Pts',(-7.7365,-1.25469068744454,0.538107958886544));
#17681=CARTESIAN_POINT('Ctrl Pts',(-7.7365,-1.23664997241023,0.589903525989738));
#17682=CARTESIAN_POINT('Ctrl Pts',(-7.7365,-1.21564557967939,0.640497721438812));
#17683=CARTESIAN_POINT('Ctrl Pts',(-7.7365,-1.19418321507496,0.692195053683102));
#17684=CARTESIAN_POINT('Ctrl Pts',(-7.7365,-1.16962630514638,0.742639006673555));
#17685=CARTESIAN_POINT('Ctrl Pts',(-7.7365,-1.14217654454016,0.791579858150175));
#17686=CARTESIAN_POINT('Ctrl Pts',(-7.7365,-1.12677101513637,0.819046754393308));
#17687=CARTESIAN_POINT('Ctrl Pts',(-7.7365,-1.11045334684977,0.846040134726086));
#17688=CARTESIAN_POINT('Ctrl Pts',(-7.7365,-1.09325230130699,0.872514108250645));
#17689=CARTESIAN_POINT('Ctrl Pts',(-7.7365,-1.08168342987847,0.890319653567393));
#17690=CARTESIAN_POINT('Ctrl Pts',(-7.7365,-1.06971486463694,0.907890215817321));
#17691=CARTESIAN_POINT('Ctrl Pts',(-7.7365,-1.05735420050082,0.925211267082703));
#17692=CARTESIAN_POINT('Ctrl Pts',(-7.7365,-1.04835406887479,0.937823189838047));
#17693=CARTESIAN_POINT('Ctrl Pts',(-7.7365,-1.03914164703506,0.950308284381235));
#17694=CARTESIAN_POINT('Ctrl Pts',(-7.7365,-1.02974297658215,0.962630950059377));
#17695=CARTESIAN_POINT('Ctrl Pts',(-7.7365,-0.994436227831979,1.00892188697543));
#17696=CARTESIAN_POINT('Ctrl Pts',(-7.7365,-0.95646308818278,1.0529859052567));
#17697=CARTESIAN_POINT('Ctrl Pts',(-7.7365,-0.916048129859651,1.09456438762751));
#17698=CARTESIAN_POINT('Ctrl Pts',(-7.7365,-0.874058720315396,1.13776264878959));
#17699=CARTESIAN_POINT('Ctrl Pts',(-7.7365,-0.829433298073862,1.17827929017471));
#17700=CARTESIAN_POINT('Ctrl Pts',(-7.7365,-0.782368886781381,1.21580225379033));
#17701=CARTESIAN_POINT('Ctrl Pts',(-7.7365,-0.738128427827426,1.2510737696997));
#17702=CARTESIAN_POINT('Ctrl Pts',(-7.7365,-0.691731985554792,1.28370079840323));
#17703=CARTESIAN_POINT('Ctrl Pts',(-7.7365,-0.643305397356536,1.31339079617938));
#17704=CARTESIAN_POINT('Ctrl Pts',(-7.7365,-0.640214236454891,1.31528596500523));
#17705=CARTESIAN_POINT('Ctrl Pts',(-7.7365,-0.637114792741105,1.31716915284921));
#17706=CARTESIAN_POINT('Ctrl Pts',(-7.7365,-0.634007094575211,1.31904027763685));
#17707=CARTESIAN_POINT('Ctrl Pts',(-7.7365,-0.686089228034766,-0.959351223124441));
#17708=CARTESIAN_POINT('Ctrl Pts',(-7.71282200757802,-0.400645460942403,
-1.16063686443021));
#17709=CARTESIAN_POINT('Ctrl Pts',(-7.66292047996862,0.404068774457181,
-1.30672719507535));
#17710=CARTESIAN_POINT('Ctrl Pts',(-7.58679541717176,1.32164391460705,-0.423509280609249));
#17711=CARTESIAN_POINT('Ctrl Pts',(-7.50812481160949,1.08034427095369,0.871377146278108));
#17712=CARTESIAN_POINT('Ctrl Pts',(-7.42945420604718,-0.133733706588163,
1.38132579741601));
#17713=CARTESIAN_POINT('Ctrl Pts',(-7.36412356393198,-1.0418916265847,0.772281661640888));
#17714=CARTESIAN_POINT('Ctrl Pts',(-7.32501645700419,-1.1759714297419,0.191448115784734));
#17715=CARTESIAN_POINT('Ctrl Pts',(-7.31213288526384,-1.17589382943587,
6.05154992187017E-5));
#17716=CARTESIAN_POINT('Origin',(-7.7365,-3.28582941601228E-17,0.));
#17717=CARTESIAN_POINT('',(-7.7365,-1.4635,-1.79227059055215E-16));
#17718=CARTESIAN_POINT('Origin',(-7.7365,0.,0.));
#17719=CARTESIAN_POINT('Origin',(-7.7365,0.,0.));
#17720=CARTESIAN_POINT('',(-7.7365,0.684664424539464,-0.958295198918394));
#17721=CARTESIAN_POINT('Ctrl Pts',(-7.7365,0.635526523537867,1.32063649424652));
#17722=CARTESIAN_POINT('Ctrl Pts',(-7.7365,0.675662324545726,1.29678049687132));
#17723=CARTESIAN_POINT('Ctrl Pts',(-7.7365,0.714498513993556,1.27094851430042));
#17724=CARTESIAN_POINT('Ctrl Pts',(-7.7365,0.751863241629522,1.24313459901083));
#17725=CARTESIAN_POINT('Ctrl Pts',(-7.7365,0.79761838124666,1.20907494816116));
#17726=CARTESIAN_POINT('Ctrl Pts',(-7.7365,0.841168365500316,1.172043366427));
#17727=CARTESIAN_POINT('Ctrl Pts',(-7.7365,0.882365785843323,1.1323407093949));
#17728=CARTESIAN_POINT('Ctrl Pts',(-7.7365,0.894337253798062,1.12080360142988));
#17729=CARTESIAN_POINT('Ctrl Pts',(-7.7365,0.906109798442489,1.10904078506667));
#17730=CARTESIAN_POINT('Ctrl Pts',(-7.7365,0.917679117349396,1.09705931043964));
#17731=CARTESIAN_POINT('Ctrl Pts',(-7.7365,0.929420235508159,1.08489991623119));
#17732=CARTESIAN_POINT('Ctrl Pts',(-7.7365,0.940955256724849,1.07251147301931));
#17733=CARTESIAN_POINT('Ctrl Pts',(-7.7365,0.952259483692321,1.05992418359167));
#17734=CARTESIAN_POINT('Ctrl Pts',(-7.7365,0.990695550087743,1.01712551247765));
#17735=CARTESIAN_POINT('Ctrl Pts',(-7.7365,1.0265099806289,0.97198836055672));
#17736=CARTESIAN_POINT('Ctrl Pts',(-7.7365,1.05955705108154,0.924827743938838));
#17737=CARTESIAN_POINT('Ctrl Pts',(-7.7365,1.08185203767515,0.893011147162164));
#17738=CARTESIAN_POINT('Ctrl Pts',(-7.7365,1.10288656680039,0.860272923873848));
#17739=CARTESIAN_POINT('Ctrl Pts',(-7.7365,1.12260321028108,0.826705490119863));
#17740=CARTESIAN_POINT('Ctrl Pts',(-7.7365,1.13151746735871,0.811529036064046));
#17741=CARTESIAN_POINT('Ctrl Pts',(-7.7365,1.14016218873329,0.796183054892689));
#17742=CARTESIAN_POINT('Ctrl Pts',(-7.7365,1.14853132555903,0.780676014340111));
#17743=CARTESIAN_POINT('Ctrl Pts',(-7.7365,1.15371651111356,0.77106846647216));
#17744=CARTESIAN_POINT('Ctrl Pts',(-7.7365,1.15879588965814,0.761398888166361));
#17745=CARTESIAN_POINT('Ctrl Pts',(-7.7365,1.1637615407048,0.751682494664184));
#17746=CARTESIAN_POINT('Ctrl Pts',(-7.7365,1.18936063251987,0.701592215054026));
#17747=CARTESIAN_POINT('Ctrl Pts',(-7.7365,1.21198804521927,0.650173906188369));
#17748=CARTESIAN_POINT('Ctrl Pts',(-7.7365,1.23150471893565,0.597718969633297));
#17749=CARTESIAN_POINT('Ctrl Pts',(-7.7365,1.2505456032793,0.546542811507523));
#17750=CARTESIAN_POINT('Ctrl Pts',(-7.7365,1.26662568914227,0.494378903403244));
#17751=CARTESIAN_POINT('Ctrl Pts',(-7.7365,1.27956755855888,0.441492195363456));
#17752=CARTESIAN_POINT('Ctrl Pts',(-7.7365,1.28740987234878,0.409444726299148));
#17753=CARTESIAN_POINT('Ctrl Pts',(-7.7365,1.29409891046221,0.377131810910926));
#17754=CARTESIAN_POINT('Ctrl Pts',(-7.7365,1.29958594646738,0.34461372675715));
#17755=CARTESIAN_POINT('Ctrl Pts',(-7.7365,1.30228746124199,0.328603610420976));
#17756=CARTESIAN_POINT('Ctrl Pts',(-7.7365,1.30469749609525,0.312543786613891));
#17757=CARTESIAN_POINT('Ctrl Pts',(-7.7365,1.30680957950161,0.296441647110286));
#17758=CARTESIAN_POINT('Ctrl Pts',(-7.7365,1.30814831885088,0.286235341954064));
#17759=CARTESIAN_POINT('Ctrl Pts',(-7.7365,1.3093675450585,0.276010135619152));
#17760=CARTESIAN_POINT('Ctrl Pts',(-7.7365,1.31046487898323,0.26577397180974));
#17761=CARTESIAN_POINT('Ctrl Pts',(-7.7365,1.31610218862947,0.213187950651897));
#17762=CARTESIAN_POINT('Ctrl Pts',(-7.7365,1.31850650693356,0.160512130657276));
#17763=CARTESIAN_POINT('Ctrl Pts',(-7.7365,1.31752770333829,0.107993690563324));
#17764=CARTESIAN_POINT('Ctrl Pts',(-7.7365,1.31716603454866,0.0885880807409719));
#17765=CARTESIAN_POINT('Ctrl Pts',(-7.7365,1.31634196331213,0.069204000142364));
#17766=CARTESIAN_POINT('Ctrl Pts',(-7.7365,1.31504611373144,0.049854209528768));
#17767=CARTESIAN_POINT('Ctrl Pts',(-7.7365,1.31152658503734,-0.00269984018871856));
#17768=CARTESIAN_POINT('Ctrl Pts',(-7.7365,1.30452994593076,-0.0550026064406229));
#17769=CARTESIAN_POINT('Ctrl Pts',(-7.7365,1.29420811169353,-0.106785251320807));
#17770=CARTESIAN_POINT('Ctrl Pts',(-7.7365,1.28945298735972,-0.130640789888765));
#17771=CARTESIAN_POINT('Ctrl Pts',(-7.7365,1.28399154727714,-0.154385628993537));
#17772=CARTESIAN_POINT('Ctrl Pts',(-7.7365,1.27783584092355,-0.177991493805362));
#17773=CARTESIAN_POINT('Ctrl Pts',(-7.7365,1.27344015870932,-0.194848028887567));
#17774=CARTESIAN_POINT('Ctrl Pts',(-7.7365,1.26869042478761,-0.211633671496613));
#17775=CARTESIAN_POINT('Ctrl Pts',(-7.7365,1.26359055949064,-0.228337623457783));
#17776=CARTESIAN_POINT('Ctrl Pts',(-7.7365,1.26062482770685,-0.238051495954687));
#17777=CARTESIAN_POINT('Ctrl Pts',(-7.7365,1.25754318746128,-0.247729405397701));
#17778=CARTESIAN_POINT('Ctrl Pts',(-7.7365,1.25434848629719,-0.257365044593482));
#17779=CARTESIAN_POINT('Ctrl Pts',(-7.7365,1.23782735626646,-0.307194947268678));
#17780=CARTESIAN_POINT('Ctrl Pts',(-7.7365,1.21827446902308,-0.355935352114231));
#17781=CARTESIAN_POINT('Ctrl Pts',(-7.7365,1.19586331884282,-0.403328860609973));
#17782=CARTESIAN_POINT('Ctrl Pts',(-7.7365,1.17355664767014,-0.450501424321841));
#17783=CARTESIAN_POINT('Ctrl Pts',(-7.7365,1.14841750560847,-0.496340514203069));
#17784=CARTESIAN_POINT('Ctrl Pts',(-7.7365,1.12057781089321,-0.540559531039698));
#17785=CARTESIAN_POINT('Ctrl Pts',(-7.7365,1.10664317367144,-0.562692530852515));
#17786=CARTESIAN_POINT('Ctrl Pts',(-7.7365,1.09203142308822,-0.584419053510079));
#17787=CARTESIAN_POINT('Ctrl Pts',(-7.7365,1.07675632505549,-0.605698999841668));
#17788=CARTESIAN_POINT('Ctrl Pts',(-7.7365,1.0654995981464,-0.621380898837115));
#17789=CARTESIAN_POINT('Ctrl Pts',(-7.7365,1.05388258904147,-0.636820217291134));
#17790=CARTESIAN_POINT('Ctrl Pts',(-7.7365,1.04191030972442,-0.651999766019219));
#17791=CARTESIAN_POINT('Ctrl Pts',(-7.7365,1.03612119897676,-0.659339729142309));
#17792=CARTESIAN_POINT('Ctrl Pts',(-7.7365,1.03024956724999,-0.666618087250615));
#17793=CARTESIAN_POINT('Ctrl Pts',(-7.7365,1.02430436591076,-0.673823161713142));
#17794=CARTESIAN_POINT('Ctrl Pts',(-7.7365,0.992204746549825,-0.71272514913416));
#17795=CARTESIAN_POINT('Ctrl Pts',(-7.7365,0.957901230445239,-0.74957321341277));
#17796=CARTESIAN_POINT('Ctrl Pts',(-7.7365,0.92152517839075,-0.784115990711642));
#17797=CARTESIAN_POINT('Ctrl Pts',(-7.7365,0.885896112329949,-0.817949428503667));
#17798=CARTESIAN_POINT('Ctrl Pts',(-7.7365,0.848278005670964,-0.849571861278115));
#17799=CARTESIAN_POINT('Ctrl Pts',(-7.7365,0.808770590985111,-0.878703555606754));
#17800=CARTESIAN_POINT('Ctrl Pts',(-7.7365,0.769263176299258,-0.907835249935393));
#17801=CARTESIAN_POINT('Ctrl Pts',(-7.7365,0.727865824984928,-0.934476884924097));
#17802=CARTESIAN_POINT('Ctrl Pts',(-7.7365,0.684664424539481,-0.958295198918382));
#17803=CARTESIAN_POINT('Origin',(-7.7365,0.,0.));
#17804=CARTESIAN_POINT('Origin',(-8.66086711473615,0.,0.));
#17805=CARTESIAN_POINT('Ctrl Pts',(-7.7365,0.684664424539464,-0.958295198918394));
#17806=CARTESIAN_POINT('Ctrl Pts',(-7.71027646481257,1.00045590899587,-0.732674539205356));
#17807=CARTESIAN_POINT('Ctrl Pts',(-7.65782939443771,1.38654401896136,0.0510548484666211));
#17808=CARTESIAN_POINT('Ctrl Pts',(-7.57915878887542,0.718476098825324,
1.1884261498247));
#17809=CARTESIAN_POINT('Ctrl Pts',(-7.50048818331313,-0.596971468671329,
1.25245241149886));
#17810=CARTESIAN_POINT('Ctrl Pts',(-7.44439095860004,-1.15153259873763,
0.495303688165933));
#17811=CARTESIAN_POINT('Ctrl Pts',(-7.41451726907438,-1.17920005900012,
0.0547824536253384));
#17812=CARTESIAN_POINT('Ctrl Pts',(-7.41086711473616,-1.17877062515776,
0.00089983691722877));
#17813=CARTESIAN_POINT('Ctrl Pts',(-7.90147783942094,0.850780204044563,
-1.1908002747757));
#17814=CARTESIAN_POINT('Ctrl Pts',(-7.87525430423351,1.24319017008315,-0.910438707813255));
#17815=CARTESIAN_POINT('Ctrl Pts',(-7.82280723385863,1.72295238526848,0.0634419619875768));
#17816=CARTESIAN_POINT('Ctrl Pts',(-7.74413662829637,0.892795390049576,
1.47676643622877));
#17817=CARTESIAN_POINT('Ctrl Pts',(-7.66546602273406,-0.741810863426415,
1.5563269830003));
#17818=CARTESIAN_POINT('Ctrl Pts',(-7.58679541717177,-1.70821806364401,
0.236880057866908));
#17819=CARTESIAN_POINT('Ctrl Pts',(-7.50812481160949,-1.1369258247315,-1.2969366021893));
#17820=CARTESIAN_POINT('Ctrl Pts',(-7.42945420604719,0.458024564052897,
-1.66255611650173));
#17821=CARTESIAN_POINT('Ctrl Pts',(-7.35078360048491,1.64056958905846,-0.531703329058153));
#17822=CARTESIAN_POINT('Ctrl Pts',(-7.27211299492261,1.3461580990934,1.07799570430111));
#17823=CARTESIAN_POINT('Ctrl Pts',(-7.19344238936033,-0.160196505892506,
1.7171046833336));
#17824=CARTESIAN_POINT('Ctrl Pts',(-7.11477178379802,-1.52232074755266,
0.810370741545469));
#17825=CARTESIAN_POINT('Ctrl Pts',(-7.03610117823575,-1.51392314204059,
-0.82595286244993));
#17826=CARTESIAN_POINT('Ctrl Pts',(-6.95743057267345,-0.142557925666395,
-1.71866947855556));
#17827=CARTESIAN_POINT('Ctrl Pts',(-6.87875996711116,1.35714926820058,-1.06409649964009));
#17828=CARTESIAN_POINT('Ctrl Pts',(-6.80008936154887,1.63503300035843,0.548472256796127));
#17829=CARTESIAN_POINT('Ctrl Pts',(-6.72141875598658,0.440917246385971,
1.66725671587453));
#17830=CARTESIAN_POINT('Ctrl Pts',(-6.64274815042429,-1.15015047653549,
1.28503232716283));
#17831=CARTESIAN_POINT('Ctrl Pts',(-6.564077544862,-1.70575259846417,-0.254090632197126));
#17832=CARTESIAN_POINT('Ctrl Pts',(-6.48540693929971,-0.725687546773451,
-1.56445880480453));
#17833=CARTESIAN_POINT('Ctrl Pts',(-6.40673633373742,0.90770464862602,-1.4663649685594));
#17834=CARTESIAN_POINT('Ctrl Pts',(-6.32806572817513,1.72390203320474,-0.0481215360256416));
#17835=CARTESIAN_POINT('Ctrl Pts',(-6.24939512261284,0.98809257879479,1.41344505915252));
#17836=CARTESIAN_POINT('Ctrl Pts',(-6.17072451705055,-0.637283914981675,
1.6025052628958));
#17837=CARTESIAN_POINT('Ctrl Pts',(-6.09205391148826,-1.68892189675471,
0.348850574905169));
#17838=CARTESIAN_POINT('Ctrl Pts',(-6.01338330592596,-1.22004521199122,
-1.21886979433108));
#17839=CARTESIAN_POINT('Ctrl Pts',(-5.93471270036368,0.347222487949291,
-1.68925736416691));
#17840=CARTESIAN_POINT('Ctrl Pts',(-5.85604209480139,1.6018902472152,-0.63882824988828));
#17841=CARTESIAN_POINT('Ctrl Pts',(-5.77737148923909,1.41439681566205,0.98672972221364));
#17842=CARTESIAN_POINT('Ctrl Pts',(-5.69870088367681,-0.0464598810777479,
1.72394761428674));
#17843=CARTESIAN_POINT('Ctrl Pts',(-5.62003027811451,-1.46548934435283,
0.909117637431074));
#17844=CARTESIAN_POINT('Ctrl Pts',(-5.54135967255222,-1.56515759577583,
-0.724179257845961));
#17845=CARTESIAN_POINT('Ctrl Pts',(-5.46268906698994,-0.255734590265156,
-1.70550687964489));
#17846=CARTESIAN_POINT('Ctrl Pts',(-5.38401846142764,1.28392297834745,-1.15138858896788));
#17847=CARTESIAN_POINT('Ctrl Pts',(-5.30534785586536,1.66768119965738,0.439310042508211));
#17848=CARTESIAN_POINT('Ctrl Pts',(-5.22667725030306,0.550047481812638,
1.63450349185888));
#17849=CARTESIAN_POINT('Ctrl Pts',(-5.14800664474078,-1.06278691078792,
1.35817446574403));
#17850=CARTESIAN_POINT('Ctrl Pts',(-5.06933603917848,-1.71880791409912,
-0.1409015669634));
#17851=CARTESIAN_POINT('Ctrl Pts',(-4.99066543361619,-0.827408254686503,
-1.51312573080365));
#17852=CARTESIAN_POINT('Ctrl Pts',(-4.91199482805391,0.808896416687006,
-1.52310225665036));
#17853=CARTESIAN_POINT('Ctrl Pts',(-4.83332422249161,1.71696204580489,-0.161849406574037));
#17854=CARTESIAN_POINT('Ctrl Pts',(-4.75465361692932,1.07926882368778,1.34511438300187));
#17855=CARTESIAN_POINT('Ctrl Pts',(-4.67598301136703,-0.530076241959179,
1.64108899053431));
#17856=CARTESIAN_POINT('Ctrl Pts',(-4.59731240580474,-1.66220048327908,
0.459612282832222));
#17857=CARTESIAN_POINT('Ctrl Pts',(-4.51864180024245,-1.29786700392053,
-1.13564745289939));
#17858=CARTESIAN_POINT('Ctrl Pts',(-4.43997119468017,0.234919449652514,
-1.70849839020005));
#17859=CARTESIAN_POINT('Ctrl Pts',(-4.36130058911786,1.55621094356038,-0.743210196573115));
#17860=CARTESIAN_POINT('Ctrl Pts',(-4.28262998355559,1.47646573646414,0.891180580009837));
#17861=CARTESIAN_POINT('Ctrl Pts',(-4.20395937799329,0.0674774128713119,
1.7232529401937));
#17862=CARTESIAN_POINT('Ctrl Pts',(-4.125288772431,-1.40225995784398,1.00390283782921));
#17863=CARTESIAN_POINT('Ctrl Pts',(-4.04661816686871,-1.60956072030047,
-0.619248080154418));
#17864=CARTESIAN_POINT('Ctrl Pts',(-3.96794756130641,-0.367794663838479,
-1.68489791451942));
#17865=CARTESIAN_POINT('Ctrl Pts',(-3.88927695574414,1.20509219906104,-1.23365582279537));
#17866=CARTESIAN_POINT('Ctrl Pts',(-3.81060635018183,1.6930500513766,0.328230742601033));
#17867=CARTESIAN_POINT('Ctrl Pts',(-3.73193574461956,0.656776713900384,
1.59461539095066));
#17868=CARTESIAN_POINT('Ctrl Pts',(-3.65326513905725,-0.970784254195621,
1.42538830861477));
#17869=CARTESIAN_POINT('Ctrl Pts',(-3.57459453349497,-1.72436064040639,
-0.0270975396048894));
#17870=CARTESIAN_POINT('Ctrl Pts',(-3.49592392793268,-0.925517318188167,
-1.4551878197274));
#17871=CARTESIAN_POINT('Ctrl Pts',(-3.41725332237038,0.706557348807113,
-1.57319122129186));
#17872=CARTESIAN_POINT('Ctrl Pts',(-3.3385827168081,1.70252751172897,-0.274870790223342));
#17873=CARTESIAN_POINT('Ctrl Pts',(-3.2599121112458,1.16573406527154,1.27091226738214));
#17874=CARTESIAN_POINT('Ctrl Pts',(-3.18124150568352,-0.420554801135517,
1.67250937498041));
#17875=CARTESIAN_POINT('Ctrl Pts',(-3.10257090012123,-1.62822352850371,
0.568367758321523));
#17876=CARTESIAN_POINT('Ctrl Pts',(-3.02390029455893,-1.37002366395617,
-1.04746796454006));
#17877=CARTESIAN_POINT('Ctrl Pts',(-2.94522968899664,0.121591103545963,
-1.72028189668636));
#17878=CARTESIAN_POINT('Ctrl Pts',(-2.86655908343436,1.50373855385807,-0.844347876428985));
#17879=CARTESIAN_POINT('Ctrl Pts',(-2.78788847787206,1.53209030147049,0.791741142594091));
#17880=CARTESIAN_POINT('Ctrl Pts',(-2.70921787230978,0.181119366601109,
1.71503681353074));
#17881=CARTESIAN_POINT('Ctrl Pts',(-2.63054726674748,-1.33290817848094,
1.09430495129436));
#17882=CARTESIAN_POINT('Ctrl Pts',(-2.55187666118519,-1.64694100897837,
-0.511611887997731));
#17883=CARTESIAN_POINT('Ctrl Pts',(-2.47320605562291,-0.478243792685512,
-1.6569381617731));
#17884=CARTESIAN_POINT('Ctrl Pts',(-2.39453545006061,1.12099068518354,-1.31053092209154));
#17885=CARTESIAN_POINT('Ctrl Pts',(-2.31586484449832,1.71104872304431,0.215704968915506));
#17886=CARTESIAN_POINT('Ctrl Pts',(-2.23719423893603,0.760601079226869,
1.54779294640914));
#17887=CARTESIAN_POINT('Ctrl Pts',(-2.15852363337374,-0.874471743967447,
1.48633055233205));
#17888=CARTESIAN_POINT('Ctrl Pts',(-2.07985302781145,-1.72252427571784,
0.0869195064554992));
#17889=CARTESIAN_POINT('Ctrl Pts',(-2.00118242224916,-1.01932419303934,
-1.39107846804535));
#17890=CARTESIAN_POINT('Ctrl Pts',(-1.92251181668687,0.600633420986038,
-1.61606823145153));
#17891=CARTESIAN_POINT('Ctrl Pts',(-1.84384121112458,1.68162810247198,-0.387362415112847));
#17892=CARTESIAN_POINT('Ctrl Pts',(-1.76517060556229,1.24515253395799,1.19255397010835));
#17893=CARTESIAN_POINT('Ctrl Pts',(-1.71272353518743,0.212069491421795,
1.526252590656));
#17894=CARTESIAN_POINT('Ctrl Pts',(-1.6865,-0.26238990830909,1.43978602091337));
#17895=CARTESIAN_POINT('Ctrl Pts',(-7.84648522628062,0.795408277542863,
-1.11329858282327));
#17896=CARTESIAN_POINT('Ctrl Pts',(-7.82026169109319,1.16227874972072,-0.851183984943956));
#17897=CARTESIAN_POINT('Ctrl Pts',(-7.76781462071834,1.61081626316611,0.059312924147259));
#17898=CARTESIAN_POINT('Ctrl Pts',(-7.68914401515604,0.834688959641492,
1.38065300742741));
#17899=CARTESIAN_POINT('Ctrl Pts',(-7.61047340959375,-0.69353106517472,
1.45503545916649));
#17900=CARTESIAN_POINT('Ctrl Pts',(-7.53180280403146,-1.59704090576079,
0.221463026427322));
#17901=CARTESIAN_POINT('Ctrl Pts',(-7.45313219846917,-1.0629304815093,-1.21252716497815));
#17902=CARTESIAN_POINT('Ctrl Pts',(-7.37446159290688,0.42821462915298,-1.5543508072453));
#17903=CARTESIAN_POINT('Ctrl Pts',(-7.2957909873446,1.53379524443405,-0.497098107266011));
#17904=CARTESIAN_POINT('Ctrl Pts',(-7.2171203817823,1.25854514457433,1.00783575156133));
#17905=CARTESIAN_POINT('Ctrl Pts',(-7.13844977622001,-0.149770324009179,
1.60534915132983));
#17906=CARTESIAN_POINT('Ctrl Pts',(-7.05977917065772,-1.4232424754622,0.75762881251765));
#17907=CARTESIAN_POINT('Ctrl Pts',(-6.98110856509543,-1.41539141721697,
-0.772196791286046));
#17908=CARTESIAN_POINT('Ctrl Pts',(-6.90243795953315,-0.133279727907777,
-1.60681210388359));
#17909=CARTESIAN_POINT('Ctrl Pts',(-6.82376735397085,1.26882096769077,-0.994841158614657));
#17910=CARTESIAN_POINT('Ctrl Pts',(-6.74509674840856,1.52861899743111,0.512775651083916));
#17911=CARTESIAN_POINT('Ctrl Pts',(-6.66642614284627,0.41222071907591,1.55874547420248));
#17912=CARTESIAN_POINT('Ctrl Pts',(-6.58775553728398,-1.07529442399706,
1.20139766425729));
#17913=CARTESIAN_POINT('Ctrl Pts',(-6.50908493172169,-1.59473590218558,
-0.237553472841633));
#17914=CARTESIAN_POINT('Ctrl Pts',(-6.4304143261594,-0.678457113681425,
-1.4626380318919));
#17915=CARTESIAN_POINT('Ctrl Pts',(-6.35174372059711,0.84862786845409,-1.37092850579528));
#17916=CARTESIAN_POINT('Ctrl Pts',(-6.27307311503482,1.6117041044977,-0.0449896082453522));
#17917=CARTESIAN_POINT('Ctrl Pts',(-6.19440250947253,0.923783854414734,
1.32145282007889));
#17918=CARTESIAN_POINT('Ctrl Pts',(-6.11573190391023,-0.595807117645157,
1.49820828558741));
#17919=CARTESIAN_POINT('Ctrl Pts',(-6.03706129834795,-1.57900060487505,
0.326146087539453));
#17920=CARTESIAN_POINT('Ctrl Pts',(-5.95839069278565,-1.14064015121761,
-1.13954123409191));
#17921=CARTESIAN_POINT('Ctrl Pts',(-5.87972008722336,0.324623962512216,
-1.57931423882567));
#17922=CARTESIAN_POINT('Ctrl Pts',(-5.80104948166108,1.49763329740499,-0.59725094151666));
#17923=CARTESIAN_POINT('Ctrl Pts',(-5.72237887609879,1.32234263274998,0.922509697587169));
#17924=CARTESIAN_POINT('Ctrl Pts',(-5.64370827053649,-0.0434360999553401,
1.61174671899407));
#17925=CARTESIAN_POINT('Ctrl Pts',(-5.5650376649742,-1.37010987045491,0.849948894714764));
#17926=CARTESIAN_POINT('Ctrl Pts',(-5.48636705941192,-1.46329134295885,
-0.677046989783222));
#17927=CARTESIAN_POINT('Ctrl Pts',(-5.40769645384962,-0.239090436030262,
-1.59450617565708));
#17928=CARTESIAN_POINT('Ctrl Pts',(-5.32902584828734,1.20036051597124,-1.07645195548704));
#17929=CARTESIAN_POINT('Ctrl Pts',(-5.25035524272504,1.55914233100869,0.410718117978727));
#17930=CARTESIAN_POINT('Ctrl Pts',(-5.17168463716275,0.51424835462257,1.52812395130572));
#17931=CARTESIAN_POINT('Ctrl Pts',(-5.09301403160046,-0.993616802654991,
1.26977944158132));
#17932=CARTESIAN_POINT('Ctrl Pts',(-5.01434342603817,-1.6069415295293,-0.131731171163432));
#17933=CARTESIAN_POINT('Ctrl Pts',(-4.93567282047588,-0.773557461205876,
-1.41464590445651));
#17934=CARTESIAN_POINT('Ctrl Pts',(-4.85700221491359,0.756250442181078,
-1.42397312105354));
#17935=CARTESIAN_POINT('Ctrl Pts',(-4.7783316093513,1.60521579717974,-0.151315647792904));
#17936=CARTESIAN_POINT('Ctrl Pts',(-4.69966100378901,1.00902601162336,1.2575693573914));
#17937=CARTESIAN_POINT('Ctrl Pts',(-4.62099039822673,-0.495576917021291,
1.53428084133828));
#17938=CARTESIAN_POINT('Ctrl Pts',(-4.54231979266443,-1.55401831994985,
0.429699013314095));
#17939=CARTESIAN_POINT('Ctrl Pts',(-4.46364918710214,-1.213397012719,-1.06173531085042));
#17940=CARTESIAN_POINT('Ctrl Pts',(-4.38497858153985,0.219630021856553,
-1.59730298762639));
#17941=CARTESIAN_POINT('Ctrl Pts',(-4.30630797597756,1.45492697200307,-0.694839324537859));
#17942=CARTESIAN_POINT('Ctrl Pts',(-4.22763737041527,1.38037187831708,0.833179247419522));
#17943=CARTESIAN_POINT('Ctrl Pts',(-4.14896676485298,0.0630857329423726,
1.6110972568637));
#17944=CARTESIAN_POINT('Ctrl Pts',(-4.07029615929069,-1.31099568658697,
0.938565123238685));
#17945=CARTESIAN_POINT('Ctrl Pts',(-3.9916255537284,-1.50480454769464,-0.578945121743281));
#17946=CARTESIAN_POINT('Ctrl Pts',(-3.91295494816611,-0.343857225006483,
-1.57523851830625));
#17947=CARTESIAN_POINT('Ctrl Pts',(-3.83428434260382,1.12666033574668,-1.15336493306441));
#17948=CARTESIAN_POINT('Ctrl Pts',(-3.75561373704152,1.58286008390573,0.306868270286214));
#17949=CARTESIAN_POINT('Ctrl Pts',(-3.67694313147924,0.614031253019605,
1.49083191572821));
#17950=CARTESIAN_POINT('Ctrl Pts',(-3.59827252591694,-0.907602019681017,
1.33261875863488));
#17951=CARTESIAN_POINT('Ctrl Pts',(-3.51960192035466,-1.61213286384424,
-0.02533393137301));
#17952=CARTESIAN_POINT('Ctrl Pts',(-3.44093131479236,-0.86528122351278,
-1.36047880720329));
#17953=CARTESIAN_POINT('Ctrl Pts',(-3.36226070923008,0.660571979846494,
-1.47080211037416));
#17954=CARTESIAN_POINT('Ctrl Pts',(-3.28359010366778,1.59172071603906,-0.256981181225197));
#17955=CARTESIAN_POINT('Ctrl Pts',(-3.20491949810549,1.0898637750651,1.18819659026007));
#17956=CARTESIAN_POINT('Ctrl Pts',(-3.12624889254321,-0.393183537173681,
1.56365627080078));
#17957=CARTESIAN_POINT('Ctrl Pts',(-3.04757828698091,-1.52225271122323,
0.531376279688018));
#17958=CARTESIAN_POINT('Ctrl Pts',(-2.96890768141862,-1.28085745009089,
-0.979294870161908));
#17959=CARTESIAN_POINT('Ctrl Pts',(-2.89023707585633,0.113677504220552,
-1.60831957987093));
#17960=CARTESIAN_POINT('Ctrl Pts',(-2.81156647029404,1.40586967975149,-0.789394589630305));
#17961=CARTESIAN_POINT('Ctrl Pts',(-2.73289586473175,1.43237619062999,0.74021169685984));
#17962=CARTESIAN_POINT('Ctrl Pts',(-2.65422525916947,0.169331447456067,
1.60341586615199));
#17963=CARTESIAN_POINT('Ctrl Pts',(-2.57555465360717,-1.24615757786577,
1.02308353235976));
#17964=CARTESIAN_POINT('Ctrl Pts',(-2.49688404804488,-1.53975198874934,
-0.478314291597477));
#17965=CARTESIAN_POINT('Ctrl Pts',(-2.41821344248259,-0.447117915505253,
-1.54909848981622));
#17966=CARTESIAN_POINT('Ctrl Pts',(-2.3395428369203,1.04803245985813,-1.22523671619525));
#17967=CARTESIAN_POINT('Ctrl Pts',(-2.26087223135801,1.59968733536411,0.201666090685789));
#17968=CARTESIAN_POINT('Ctrl Pts',(-2.18220162579572,0.71109834414223,1.44705684928207));
#17969=CARTESIAN_POINT('Ctrl Pts',(-2.10353102023343,-0.817557884307119,
1.38959465543445));
#17970=CARTESIAN_POINT('Ctrl Pts',(-2.02486041467114,-1.61041601657051,
0.0812624630732668));
#17971=CARTESIAN_POINT('Ctrl Pts',(-1.94618980910885,-0.95298279953951,
-1.30054192955453));
#17972=CARTESIAN_POINT('Ctrl Pts',(-1.86751920354656,0.561541973532051,
-1.51088852591975));
#17973=CARTESIAN_POINT('Ctrl Pts',(-1.78884859798427,1.57218151773645,-0.362151434559715));
#17974=CARTESIAN_POINT('Ctrl Pts',(-1.71017799242198,1.16411339568706,1.11493814116895));
#17975=CARTESIAN_POINT('Ctrl Pts',(-1.65773092204712,0.198267223531165,
1.42691841965499));
#17976=CARTESIAN_POINT('Ctrl Pts',(-1.63150738685969,-0.245312601328269,
1.34607941449588));
#17977=CARTESIAN_POINT('Ctrl Pts',(-7.79149261314031,0.740036351041164,
-1.03579689087083));
#17978=CARTESIAN_POINT('Ctrl Pts',(-7.76526907795288,1.08136732935829,-0.791929262074656));
#17979=CARTESIAN_POINT('Ctrl Pts',(-7.71282200757803,1.49868014106374,0.0551838863069402));
#17980=CARTESIAN_POINT('Ctrl Pts',(-7.63415140201572,0.776582529233407,
1.28453957862605));
#17981=CARTESIAN_POINT('Ctrl Pts',(-7.55548079645345,-0.645251266923024,
1.35374393533268));
#17982=CARTESIAN_POINT('Ctrl Pts',(-7.47681019089115,-1.48586374787757,
0.206045994987737));
#17983=CARTESIAN_POINT('Ctrl Pts',(-7.39813958532887,-0.98893513828711,
-1.128117727767));
#17984=CARTESIAN_POINT('Ctrl Pts',(-7.31946897976657,0.398404694253064,
-1.44614549798886));
#17985=CARTESIAN_POINT('Ctrl Pts',(-7.24079837420428,1.42702089980965,-0.462492885473871));
#17986=CARTESIAN_POINT('Ctrl Pts',(-7.16212776864199,1.17093219005527,0.937675798821544));
#17987=CARTESIAN_POINT('Ctrl Pts',(-7.0834571630797,-0.13934414212585,1.49359361932605));
#17988=CARTESIAN_POINT('Ctrl Pts',(-7.0047865575174,-1.32416420337174,0.704886883489828));
#17989=CARTESIAN_POINT('Ctrl Pts',(-6.92611595195512,-1.31685969239335,
-0.718440720122158));
#17990=CARTESIAN_POINT('Ctrl Pts',(-6.84744534639283,-0.124001530149162,
-1.49495472921164));
#17991=CARTESIAN_POINT('Ctrl Pts',(-6.76877474083054,1.18049266718097,-0.925585817589218));
#17992=CARTESIAN_POINT('Ctrl Pts',(-6.69010413526825,1.42220499450378,0.477079045371704));
#17993=CARTESIAN_POINT('Ctrl Pts',(-6.61143352970596,0.383524191765849,
1.45023423253043));
#17994=CARTESIAN_POINT('Ctrl Pts',(-6.53276292414367,-1.00043837145862,
1.11776300135174));
#17995=CARTESIAN_POINT('Ctrl Pts',(-6.45409231858137,-1.48371920590699,
-0.221016313486138));
#17996=CARTESIAN_POINT('Ctrl Pts',(-6.37542171301909,-0.631226680589397,
-1.36081725897928));
#17997=CARTESIAN_POINT('Ctrl Pts',(-6.29675110745679,0.789551088282159,
-1.27549204303116));
#17998=CARTESIAN_POINT('Ctrl Pts',(-6.21808050189452,1.49950617579067,-0.0418576804650646));
#17999=CARTESIAN_POINT('Ctrl Pts',(-6.13940989633221,0.859475130034677,
1.22946058100525));
#18000=CARTESIAN_POINT('Ctrl Pts',(-6.06073929076993,-0.554330320308637,
1.39391130827902));
#18001=CARTESIAN_POINT('Ctrl Pts',(-5.98206868520763,-1.46907931299539,
0.303441600173735));
#18002=CARTESIAN_POINT('Ctrl Pts',(-5.90339807964535,-1.06123509044401,
-1.06021267385274));
#18003=CARTESIAN_POINT('Ctrl Pts',(-5.82472747408305,0.302025437075139,
-1.46937111348443));
#18004=CARTESIAN_POINT('Ctrl Pts',(-5.74605686852076,1.39337634759478,-0.555673633145038));
#18005=CARTESIAN_POINT('Ctrl Pts',(-5.66738626295848,1.2302884498379,0.858289672960698));
#18006=CARTESIAN_POINT('Ctrl Pts',(-5.58871565739618,-0.0404123188329307,
1.49954582370141));
#18007=CARTESIAN_POINT('Ctrl Pts',(-5.51004505183389,-1.27473039655699,
0.790780151998455));
#18008=CARTESIAN_POINT('Ctrl Pts',(-5.4313744462716,-1.36142509014187,-0.629914721720484));
#18009=CARTESIAN_POINT('Ctrl Pts',(-5.35270384070931,-0.222446281795369,
-1.48350547166926));
#18010=CARTESIAN_POINT('Ctrl Pts',(-5.27403323514702,1.11679805359503,-1.00151532200621));
#18011=CARTESIAN_POINT('Ctrl Pts',(-5.19536262958473,1.45060346235999,0.382126193449246));
#18012=CARTESIAN_POINT('Ctrl Pts',(-5.11669202402245,0.478449227432503,
1.42174441075256));
#18013=CARTESIAN_POINT('Ctrl Pts',(-5.03802141846014,-0.924446694522063,
1.18138441741861));
#18014=CARTESIAN_POINT('Ctrl Pts',(-4.95935081289786,-1.49507514495947,
-0.122560775363463));
#18015=CARTESIAN_POINT('Ctrl Pts',(-4.88068020733557,-0.719706667725249,
-1.31616607810937));
#18016=CARTESIAN_POINT('Ctrl Pts',(-4.80200960177328,0.703604467675148,
-1.32484398545671));
#18017=CARTESIAN_POINT('Ctrl Pts',(-4.72333899621099,1.49346954855458,-0.140781889011772));
#18018=CARTESIAN_POINT('Ctrl Pts',(-4.6446683906487,0.938783199558951,1.17002433178093));
#18019=CARTESIAN_POINT('Ctrl Pts',(-4.56599778508641,-0.461077592083401,
1.42747269214224));
#18020=CARTESIAN_POINT('Ctrl Pts',(-4.48732717952412,-1.44583615662062,
0.399785743795968));
#18021=CARTESIAN_POINT('Ctrl Pts',(-4.40865657396183,-1.12892702151747,
-0.98782316880146));
#18022=CARTESIAN_POINT('Ctrl Pts',(-4.32998596839954,0.204340594060589,
-1.48610758505272));
#18023=CARTESIAN_POINT('Ctrl Pts',(-4.25131536283724,1.35364300044576,-0.6464684525026));
#18024=CARTESIAN_POINT('Ctrl Pts',(-4.17264475727496,1.28427802017003,0.775177914829204));
#18025=CARTESIAN_POINT('Ctrl Pts',(-4.09397415171266,0.0586940530134323,
1.49894157353371));
#18026=CARTESIAN_POINT('Ctrl Pts',(-4.01530354615037,-1.21973141532996,
0.873227408648153));
#18027=CARTESIAN_POINT('Ctrl Pts',(-3.93663294058809,-1.40004837508882,
-0.538642163332144));
#18028=CARTESIAN_POINT('Ctrl Pts',(-3.85796233502579,-0.319919786174487,
-1.46557912209308));
#18029=CARTESIAN_POINT('Ctrl Pts',(-3.7792917294635,1.04822847243233,-1.07307404333344));
#18030=CARTESIAN_POINT('Ctrl Pts',(-3.70062112390122,1.47267011643486,0.285505797971395));
#18031=CARTESIAN_POINT('Ctrl Pts',(-3.62195051833892,0.571285792138825,
1.38704844050577));
#18032=CARTESIAN_POINT('Ctrl Pts',(-3.54327991277664,-0.844419785166412,
1.239849208655));
#18033=CARTESIAN_POINT('Ctrl Pts',(-3.46460930721434,-1.49990508728209,
-0.0235703231411309));
#18034=CARTESIAN_POINT('Ctrl Pts',(-3.38593870165205,-0.80504512883739,
-1.26576979467919));
#18035=CARTESIAN_POINT('Ctrl Pts',(-3.30726809608976,0.614586610885873,
-1.36841299945646));
#18036=CARTESIAN_POINT('Ctrl Pts',(-3.22859749052747,1.48091392034915,-0.239091572227054));
#18037=CARTESIAN_POINT('Ctrl Pts',(-3.14992688496518,1.01399348485866,1.10548091313801));
#18038=CARTESIAN_POINT('Ctrl Pts',(-3.07125627940289,-0.365812273211845,
1.45480316662115));
#18039=CARTESIAN_POINT('Ctrl Pts',(-2.9925856738406,-1.41628189394276,0.494384801054513));
#18040=CARTESIAN_POINT('Ctrl Pts',(-2.91391506827831,-1.19169123622562,
-0.911121775783751));
#18041=CARTESIAN_POINT('Ctrl Pts',(-2.83524446271602,0.105763904895138,
-1.49635726305551));
#18042=CARTESIAN_POINT('Ctrl Pts',(-2.75657385715373,1.30800080564492,-0.734441302831623));
#18043=CARTESIAN_POINT('Ctrl Pts',(-2.67790325159144,1.33266207978949,0.688682251125587));
#18044=CARTESIAN_POINT('Ctrl Pts',(-2.59923264602915,0.157543528311028,
1.49179491877324));
#18045=CARTESIAN_POINT('Ctrl Pts',(-2.52056204046686,-1.1594069772506,0.951862113425152));
#18046=CARTESIAN_POINT('Ctrl Pts',(-2.44189143490457,-1.4325629685203,-0.445016695197221));
#18047=CARTESIAN_POINT('Ctrl Pts',(-2.36322082934228,-0.415992038324998,
-1.44125881785935));
#18048=CARTESIAN_POINT('Ctrl Pts',(-2.28455022377999,0.975074234532735,
-1.13994251029895));
#18049=CARTESIAN_POINT('Ctrl Pts',(-2.2058796182177,1.48832594768391,0.187627212456071));
#18050=CARTESIAN_POINT('Ctrl Pts',(-2.12720901265541,0.661595609057591,
1.346320752155));
#18051=CARTESIAN_POINT('Ctrl Pts',(-2.04853840709312,-0.76064402464679,
1.29285875853686));
#18052=CARTESIAN_POINT('Ctrl Pts',(-1.96986780153083,-1.49830775742317,
0.0756054196910335));
#18053=CARTESIAN_POINT('Ctrl Pts',(-1.89119719596854,-0.886641406039676,
-1.21000539106371));
#18054=CARTESIAN_POINT('Ctrl Pts',(-1.81252659040624,0.522450526078063,
-1.40570882038797));
#18055=CARTESIAN_POINT('Ctrl Pts',(-1.73385598484396,1.46273493300092,-0.336940454006583));
#18056=CARTESIAN_POINT('Ctrl Pts',(-1.65518537928166,1.08307425741613,1.03732231222955));
#18057=CARTESIAN_POINT('Ctrl Pts',(-1.60273830890681,0.184464955640538,
1.32758424865397));
#18058=CARTESIAN_POINT('Ctrl Pts',(-1.57651477371938,-0.228235294347447,
1.25237280807838));
#18059=CARTESIAN_POINT('Ctrl Pts',(-7.7365,0.684664424539464,-0.958295198918394));
#18060=CARTESIAN_POINT('Ctrl Pts',(-7.71027646481257,1.00045590899587,-0.732674539205356));
#18061=CARTESIAN_POINT('Ctrl Pts',(-7.65782939443771,1.38654401896136,0.0510548484666211));
#18062=CARTESIAN_POINT('Ctrl Pts',(-7.57915878887542,0.718476098825324,
1.1884261498247));
#18063=CARTESIAN_POINT('Ctrl Pts',(-7.50048818331313,-0.596971468671329,
1.25245241149886));
#18064=CARTESIAN_POINT('Ctrl Pts',(-7.42181757775084,-1.37468658999435,
0.190628963548152));
#18065=CARTESIAN_POINT('Ctrl Pts',(-7.34314697218855,-0.914939795064915,
-1.04370829055584));
#18066=CARTESIAN_POINT('Ctrl Pts',(-7.26447636662626,0.368594759353147,
-1.33794018873242));
#18067=CARTESIAN_POINT('Ctrl Pts',(-7.18580576106397,1.32024655518524,-0.427887663681729));
#18068=CARTESIAN_POINT('Ctrl Pts',(-7.10713515550168,1.0833192355362,0.867515846081762));
#18069=CARTESIAN_POINT('Ctrl Pts',(-7.02846454993939,-0.128917960242522,
1.38183808732227));
#18070=CARTESIAN_POINT('Ctrl Pts',(-6.94979394437709,-1.22508593128128,
0.652144954462008));
#18071=CARTESIAN_POINT('Ctrl Pts',(-6.87112333881481,-1.21832796756972,
-0.664684648958273));
#18072=CARTESIAN_POINT('Ctrl Pts',(-6.79245273325251,-0.114723332390545,
-1.38309735453967));
#18073=CARTESIAN_POINT('Ctrl Pts',(-6.71378212769023,1.09216436667117,-0.856330476563782));
#18074=CARTESIAN_POINT('Ctrl Pts',(-6.63511152212794,1.31579099157645,0.441382439659493));
#18075=CARTESIAN_POINT('Ctrl Pts',(-6.55644091656565,0.354827664455788,
1.34172299085838));
#18076=CARTESIAN_POINT('Ctrl Pts',(-6.47777031100335,-0.92558231892019,
1.0341283384462));
#18077=CARTESIAN_POINT('Ctrl Pts',(-6.39909970544107,-1.37270250962841,
-0.204479154130645));
#18078=CARTESIAN_POINT('Ctrl Pts',(-6.32042909987877,-0.583996247497372,
-1.25899648606665));
#18079=CARTESIAN_POINT('Ctrl Pts',(-6.24175849431649,0.73047430811023,-1.18005558026704));
#18080=CARTESIAN_POINT('Ctrl Pts',(-6.1630878887542,1.38730824708363,-0.0387257526847742));
#18081=CARTESIAN_POINT('Ctrl Pts',(-6.0844172831919,0.795166405654621,1.1374683419316));
#18082=CARTESIAN_POINT('Ctrl Pts',(-6.00574667762961,-0.512853522972119,
1.28961433097063));
#18083=CARTESIAN_POINT('Ctrl Pts',(-5.92707607206732,-1.35915802111573,
0.280737112808016));
#18084=CARTESIAN_POINT('Ctrl Pts',(-5.84840546650503,-0.981830029670403,
-0.980884113613565));
#18085=CARTESIAN_POINT('Ctrl Pts',(-5.76973486094274,0.279426911638065,
-1.3594279881432));
#18086=CARTESIAN_POINT('Ctrl Pts',(-5.69106425538045,1.28911939778457,-0.514096324773416));
#18087=CARTESIAN_POINT('Ctrl Pts',(-5.61239364981816,1.13823426692583,0.794069648334226));
#18088=CARTESIAN_POINT('Ctrl Pts',(-5.53372304425587,-0.0373885377105224,
1.38734492840875));
#18089=CARTESIAN_POINT('Ctrl Pts',(-5.45505243869358,-1.17935092265908,
0.731611409282145));
#18090=CARTESIAN_POINT('Ctrl Pts',(-5.37638183313129,-1.25955883732489,
-0.582782453657743));
#18091=CARTESIAN_POINT('Ctrl Pts',(-5.297711227569,-0.205802127560476,-1.37250476768144));
#18092=CARTESIAN_POINT('Ctrl Pts',(-5.21904062200671,1.03323559121881,-0.926578688525379));
#18093=CARTESIAN_POINT('Ctrl Pts',(-5.14037001644442,1.34206459371129,0.353534268919763));
#18094=CARTESIAN_POINT('Ctrl Pts',(-5.06169941088212,0.442650100242435,
1.31536487019939));
#18095=CARTESIAN_POINT('Ctrl Pts',(-4.98302880531984,-0.855276586389133,
1.0929893932559));
#18096=CARTESIAN_POINT('Ctrl Pts',(-4.90435819975755,-1.38320876038964,
-0.113390379563494));
#18097=CARTESIAN_POINT('Ctrl Pts',(-4.82568759419526,-0.66585587424462,
-1.21768625176223));
#18098=CARTESIAN_POINT('Ctrl Pts',(-4.74701698863296,0.650958493169218,
-1.22571484985989));
#18099=CARTESIAN_POINT('Ctrl Pts',(-4.66834638307068,1.38172329992943,-0.130248130230639));
#18100=CARTESIAN_POINT('Ctrl Pts',(-4.58967577750838,0.868540387494536,
1.08247930617046));
#18101=CARTESIAN_POINT('Ctrl Pts',(-4.5110051719461,-0.42657826714551,1.32066454294621));
#18102=CARTESIAN_POINT('Ctrl Pts',(-4.4323345663838,-1.33765399329139,0.36987247427784));
#18103=CARTESIAN_POINT('Ctrl Pts',(-4.35366396082152,-1.04445703031594,
-0.913911026752496));
#18104=CARTESIAN_POINT('Ctrl Pts',(-4.27499335525923,0.189051166264626,
-1.37491218247906));
#18105=CARTESIAN_POINT('Ctrl Pts',(-4.19632274969693,1.25235902888845,-0.598097580467343));
#18106=CARTESIAN_POINT('Ctrl Pts',(-4.11765214413465,1.18818416202297,0.717176582238888));
#18107=CARTESIAN_POINT('Ctrl Pts',(-4.03898153857235,0.0543023730844936,
1.38678589020371));
#18108=CARTESIAN_POINT('Ctrl Pts',(-3.96031093301006,-1.12846714407295,
0.807889694057623));
#18109=CARTESIAN_POINT('Ctrl Pts',(-3.88164032744778,-1.295292202483,-0.498339204921006));
#18110=CARTESIAN_POINT('Ctrl Pts',(-3.80296972188548,-0.295982347342492,
-1.35591972587991));
#18111=CARTESIAN_POINT('Ctrl Pts',(-3.72429911632319,0.969796609117977,
-0.992783153602477));
#18112=CARTESIAN_POINT('Ctrl Pts',(-3.6456285107609,1.36248014896398,0.264143325656574));
#18113=CARTESIAN_POINT('Ctrl Pts',(-3.56695790519861,0.528540331258045,
1.28326496528333));
#18114=CARTESIAN_POINT('Ctrl Pts',(-3.48828729963633,-0.781237550651807,
1.14707965867511));
#18115=CARTESIAN_POINT('Ctrl Pts',(-3.40961669407403,-1.38767731071994,
-0.0218067149092513));
#18116=CARTESIAN_POINT('Ctrl Pts',(-3.33094608851175,-0.744809034162001,
-1.17106078215508));
#18117=CARTESIAN_POINT('Ctrl Pts',(-3.25227548294945,0.568601241925253,
-1.26602388853876));
#18118=CARTESIAN_POINT('Ctrl Pts',(-3.17360487738716,1.37010712465924,-0.22120196322891));
#18119=CARTESIAN_POINT('Ctrl Pts',(-3.09493427182487,0.938123194652226,
1.02276523601594));
#18120=CARTESIAN_POINT('Ctrl Pts',(-3.01626366626258,-0.338441009250009,
1.34595006244152));
#18121=CARTESIAN_POINT('Ctrl Pts',(-2.93759306070029,-1.31031107666228,
0.457393322421008));
#18122=CARTESIAN_POINT('Ctrl Pts',(-2.858922455138,-1.10252502236034,-0.842948681405594));
#18123=CARTESIAN_POINT('Ctrl Pts',(-2.78025184957571,0.0978503055697247,
-1.38439494624008));
#18124=CARTESIAN_POINT('Ctrl Pts',(-2.70158124401342,1.21013193153834,-0.679488016032942));
#18125=CARTESIAN_POINT('Ctrl Pts',(-2.62291063845113,1.232947968949,0.637152805391334));
#18126=CARTESIAN_POINT('Ctrl Pts',(-2.54424003288884,0.145755609165987,
1.38017397139449));
#18127=CARTESIAN_POINT('Ctrl Pts',(-2.46556942732655,-1.07265637663543,
0.880640694490544));
#18128=CARTESIAN_POINT('Ctrl Pts',(-2.38689882176426,-1.32537394829127,
-0.411719098796964));
#18129=CARTESIAN_POINT('Ctrl Pts',(-2.30822821620197,-0.384866161144742,
-1.33341914590248));
#18130=CARTESIAN_POINT('Ctrl Pts',(-2.22955761063968,0.902116009207335,
-1.05464830440266));
#18131=CARTESIAN_POINT('Ctrl Pts',(-2.15088700507739,1.37696456000371,0.173588334226353));
#18132=CARTESIAN_POINT('Ctrl Pts',(-2.0722163995151,0.612092873972952,1.24558465502793));
#18133=CARTESIAN_POINT('Ctrl Pts',(-1.9935457939528,-0.703730164986462,
1.19612286163926));
#18134=CARTESIAN_POINT('Ctrl Pts',(-1.91487518839052,-1.38619949827584,
0.069948376308802));
#18135=CARTESIAN_POINT('Ctrl Pts',(-1.83620458282822,-0.820300012539843,
-1.11946885257289));
#18136=CARTESIAN_POINT('Ctrl Pts',(-1.75753397726593,0.483359078624077,
-1.30052911485619));
#18137=CARTESIAN_POINT('Ctrl Pts',(-1.67886337170364,1.35328834826538,-0.31172947345345));
#18138=CARTESIAN_POINT('Ctrl Pts',(-1.60019276614135,1.0020351191452,0.959706483290145));
#18139=CARTESIAN_POINT('Ctrl Pts',(-1.54774569576649,0.170662687749908,
1.22825007765296));
#18140=CARTESIAN_POINT('Ctrl Pts',(-1.52152216057906,-0.211157987366626,
1.15866620166089));
#18141=CARTESIAN_POINT('Ctrl Pts',(-1.6865,-0.262389908309069,1.43978602091337));
#18142=CARTESIAN_POINT('Ctrl Pts',(-1.71272353518743,0.212069491421808,
1.52625259065599));
#18143=CARTESIAN_POINT('Ctrl Pts',(-1.73894707037486,0.728611012689902,
1.35940328038217));
#18144=CARTESIAN_POINT('Ctrl Pts',(-1.76517060556229,1.05962770140961,1.01265922770839));
#18145=CARTESIAN_POINT('Ctrl Pts',(-1.79139414074972,1.39064439012933,0.665915175034609));
#18146=CARTESIAN_POINT('Ctrl Pts',(-1.81761767593715,1.53613624630066,0.139276379960869));
#18147=CARTESIAN_POINT('Ctrl Pts',(-1.84384121112458,1.42871639413866,-0.328827320299109));
#18148=CARTESIAN_POINT('Ctrl Pts',(-1.87006474631201,1.32129654197666,-0.796931020559087));
#18149=CARTESIAN_POINT('Ctrl Pts',(-1.89628828149944,0.960964981481353,
-1.2064996260053));
#18150=CARTESIAN_POINT('Ctrl Pts',(-1.92251181668687,0.510806265562799,
-1.37378563482738));
#18151=CARTESIAN_POINT('Ctrl Pts',(-1.9487353518743,0.0606475496442437,
-1.54107164364947));
#18152=CARTESIAN_POINT('Ctrl Pts',(-1.97495888706173,-0.479338321697556,
-1.46607505584741));
#18153=CARTESIAN_POINT('Ctrl Pts',(-2.00118242224916,-0.866531271148201,
-1.18224376619624));
#18154=CARTESIAN_POINT('Ctrl Pts',(-2.02606993288514,-1.23399769315247,
-0.912872981916841));
#18155=CARTESIAN_POINT('Ctrl Pts',(-2.05095744352111,-1.46384344241319,
-0.455404661410297));
#18156=CARTESIAN_POINT('Ctrl Pts',(-2.07584495415709,-1.46567283994288,
0.000450589203851749));
#18157=CARTESIAN_POINT('Origin',(-1.69543030951378,0.,0.));
#18158=CARTESIAN_POINT('',(-2.00086061902756,0.,0.));
#18159=CARTESIAN_POINT('',(-1.4,-0.983629653494575,1.20459890669855E-16));
#18160=CARTESIAN_POINT('',(-1.69543030951378,-0.5,-6.12323399573677E-17));
#18161=CARTESIAN_POINT('Origin',(-1.4,0.,0.));
#18162=CARTESIAN_POINT('Origin',(0.,1.38777878078145E-16,1.15470053837925));
#18163=CARTESIAN_POINT('',(0.,7.07050159149938E-17,1.15470053837925));
#18164=CARTESIAN_POINT('',(0.,1.,0.577350269189626));
#18165=CARTESIAN_POINT('',(0.,0.25,1.01036297108185));
#18166=CARTESIAN_POINT('',(-1.4,1.38777878078145E-16,1.15470053837925));
#18167=CARTESIAN_POINT('',(0.,7.07050159149938E-17,1.15470053837925));
#18168=CARTESIAN_POINT('',(-1.4,1.,0.577350269189626));
#18169=CARTESIAN_POINT('',(-1.4,1.,0.577350269189626));
#18170=CARTESIAN_POINT('',(0.,1.,0.577350269189626));
#18171=CARTESIAN_POINT('Origin',(0.,-1.,0.577350269189626));
#18172=CARTESIAN_POINT('',(0.,-1.,0.577350269189626));
#18173=CARTESIAN_POINT('',(0.,-0.75,0.721687836487032));
#18174=CARTESIAN_POINT('',(-1.4,-1.,0.577350269189626));
#18175=CARTESIAN_POINT('',(0.,-1.,0.577350269189626));
#18176=CARTESIAN_POINT('',(-1.4,7.07050159149938E-17,1.15470053837925));
#18177=CARTESIAN_POINT('Origin',(0.,-1.,-0.577350269189626));
#18178=CARTESIAN_POINT('',(0.,-1.,-0.577350269189626));
#18179=CARTESIAN_POINT('',(0.,-1.,-0.288675134594813));
#18180=CARTESIAN_POINT('',(-1.4,-1.,-0.577350269189626));
#18181=CARTESIAN_POINT('',(0.,-1.,-0.577350269189626));
#18182=CARTESIAN_POINT('',(-1.4,-1.,0.577350269189626));
#18183=CARTESIAN_POINT('Origin',(0.,-2.77555756156289E-16,-1.15470053837925));
#18184=CARTESIAN_POINT('',(0.,-2.12115047744981E-16,-1.15470053837925));
#18185=CARTESIAN_POINT('',(0.,-0.25,-1.01036297108185));
#18186=CARTESIAN_POINT('',(-1.4,-2.77555756156289E-16,-1.15470053837925));
#18187=CARTESIAN_POINT('',(0.,-2.12115047744981E-16,-1.15470053837925));
#18188=CARTESIAN_POINT('',(-1.4,-1.,-0.577350269189626));
#18189=CARTESIAN_POINT('Origin',(0.,1.,-0.577350269189626));
#18190=CARTESIAN_POINT('',(0.,1.,-0.577350269189626));
#18191=CARTESIAN_POINT('',(0.,0.75,-0.721687836487033));
#18192=CARTESIAN_POINT('',(-1.4,1.,-0.577350269189626));
#18193=CARTESIAN_POINT('',(0.,1.,-0.577350269189626));
#18194=CARTESIAN_POINT('',(-1.4,-2.12115047744981E-16,-1.15470053837925));
#18195=CARTESIAN_POINT('Origin',(0.,1.,0.577350269189626));
#18196=CARTESIAN_POINT('',(0.,1.,0.288675134594813));
#18197=CARTESIAN_POINT('',(-1.4,1.,-0.577350269189626));
#18198=CARTESIAN_POINT('Origin',(-1.4,0.,0.));
#18199=CARTESIAN_POINT('Origin',(-8.,1.2,0.));
#18200=CARTESIAN_POINT('',(-8.,-1.2,-1.46957615897682E-16));
#18201=CARTESIAN_POINT('Origin',(-8.,0.,0.));
#18202=CARTESIAN_POINT('Origin',(-7.85,0.,0.));
#18203=CARTESIAN_POINT('',(-7.85,-1.35,-1.65327317884893E-16));
#18204=CARTESIAN_POINT('Origin',(-4.675,0.,0.));
#18205=CARTESIAN_POINT('Origin',(-1.6865,0.,0.));
#18206=CARTESIAN_POINT('Origin',(-0.825,0.,0.));
#18207=CARTESIAN_POINT('',(0.,-3.15,-3.85763741731416E-16));
#18208=CARTESIAN_POINT('Origin',(0.,0.,0.));
#18209=CARTESIAN_POINT('',(-0.825,-2.325,-2.8473038080176E-16));
#18210=CARTESIAN_POINT('Origin',(0.,0.,0.));
#18211=CARTESIAN_POINT('',(0.,0.,0.));
#18212=CARTESIAN_POINT('Origin',(0.,2.,0.));
#18213=CARTESIAN_POINT('',(1.73472347597681E-15,-2.,-2.4492935982947E-16));
#18214=CARTESIAN_POINT('Origin',(0.,0.,0.));
#18215=CARTESIAN_POINT('Origin',(0.250000000000004,0.,0.));
#18216=CARTESIAN_POINT('',(0.500000000000001,-2.5,-3.06161699786838E-16));
#18217=CARTESIAN_POINT('Origin',(0.499999999999998,0.,0.));
#18218=CARTESIAN_POINT('',(0.250000000000004,-2.25,-2.75545529808154E-16));
#18219=CARTESIAN_POINT('Origin',(35.,0.,0.));
#18220=CARTESIAN_POINT('',(69.5,-2.5,-3.06161699786838E-16));
#18221=CARTESIAN_POINT('Origin',(69.5,0.,0.));
#18222=CARTESIAN_POINT('',(35.,-2.5,-3.06161699786838E-16));
#18223=CARTESIAN_POINT('Origin',(69.75,0.,0.));
#18224=CARTESIAN_POINT('',(70.,-2.,-2.4492935982947E-16));
#18225=CARTESIAN_POINT('Origin',(70.,0.,0.));
#18226=CARTESIAN_POINT('',(69.75,-2.25,-2.75545529808154E-16));
#18227=CARTESIAN_POINT('Origin',(70.,0.,0.));
#18228=CARTESIAN_POINT('',(0.,0.,0.));
#18229=CARTESIAN_POINT('',(0.,0.,0.));
#18230=CARTESIAN_POINT('',(0.,0.,0.));
#18231=CARTESIAN_POINT('',(0.,0.,0.));
#18232=CARTESIAN_POINT('',(0.,0.,0.));
#18233=CARTESIAN_POINT('',(100.,0.,0.));
#18234=CARTESIAN_POINT('',(6.2,1.77635683940025E-14,47.5));
#18235=CARTESIAN_POINT('',(6.2,1.77635683940025E-14,47.5));
#18236=CARTESIAN_POINT('',(93.8,1.77635683940025E-14,47.5));
#18237=CARTESIAN_POINT('',(-3.,0.,47.5));
#18238=CARTESIAN_POINT('',(103.,0.,47.5));
#18239=CARTESIAN_POINT('',(-4.3,1.77635683940025E-14,47.5));
#18240=CARTESIAN_POINT('',(-7.8,1.11022302462516E-14,51.5));
#18241=CARTESIAN_POINT('',(-3.,-25.,26.5));
#18242=CARTESIAN_POINT('',(103.,-25.,26.5));
#18243=CARTESIAN_POINT('',(-3.,-25.,66.5));
#18244=CARTESIAN_POINT('',(103.,-25.,66.5));
#18245=CARTESIAN_POINT('',(-3.,25.,26.5));
#18246=CARTESIAN_POINT('',(103.,25.,26.5));
#18247=CARTESIAN_POINT('',(-3.,25.,66.5));
#18248=CARTESIAN_POINT('',(103.,25.,66.5));
#18249=CARTESIAN_POINT('',(20.,-35.,19.));
#18250=CARTESIAN_POINT('',(50.,-35.,19.));
#18251=CARTESIAN_POINT('',(80.,-35.,19.));
#18252=UNCERTAINTY_MEASURE_WITH_UNIT(LENGTH_MEASURE(0.01),#18282,
'DISTANCE_ACCURACY_VALUE',
'Maximum model space distance between geometric entities at asserted c
onnectivities');
#18253=UNCERTAINTY_MEASURE_WITH_UNIT(LENGTH_MEASURE(0.01),#18282,
'DISTANCE_ACCURACY_VALUE',
'Maximum model space distance between geometric entities at asserted c
onnectivities');
#18254=UNCERTAINTY_MEASURE_WITH_UNIT(LENGTH_MEASURE(0.01),#18282,
'DISTANCE_ACCURACY_VALUE',
'Maximum model space distance between geometric entities at asserted c
onnectivities');
#18255=UNCERTAINTY_MEASURE_WITH_UNIT(LENGTH_MEASURE(0.01),#18282,
'DISTANCE_ACCURACY_VALUE',
'Maximum model space distance between geometric entities at asserted c
onnectivities');
#18256=UNCERTAINTY_MEASURE_WITH_UNIT(LENGTH_MEASURE(0.01),#18282,
'DISTANCE_ACCURACY_VALUE',
'Maximum model space distance between geometric entities at asserted c
onnectivities');
#18257=UNCERTAINTY_MEASURE_WITH_UNIT(LENGTH_MEASURE(0.01),#18282,
'DISTANCE_ACCURACY_VALUE',
'Maximum model space distance between geometric entities at asserted c
onnectivities');
#18258=UNCERTAINTY_MEASURE_WITH_UNIT(LENGTH_MEASURE(0.01),#18282,
'DISTANCE_ACCURACY_VALUE',
'Maximum model space distance between geometric entities at asserted c
onnectivities');
#18259=UNCERTAINTY_MEASURE_WITH_UNIT(LENGTH_MEASURE(0.01),#18282,
'DISTANCE_ACCURACY_VALUE',
'Maximum model space distance between geometric entities at asserted c
onnectivities');
#18260=UNCERTAINTY_MEASURE_WITH_UNIT(LENGTH_MEASURE(0.01),#18282,
'DISTANCE_ACCURACY_VALUE',
'Maximum model space distance between geometric entities at asserted c
onnectivities');
#18261=UNCERTAINTY_MEASURE_WITH_UNIT(LENGTH_MEASURE(0.01),#18282,
'DISTANCE_ACCURACY_VALUE',
'Maximum model space distance between geometric entities at asserted c
onnectivities');
#18262=UNCERTAINTY_MEASURE_WITH_UNIT(LENGTH_MEASURE(0.01),#18282,
'DISTANCE_ACCURACY_VALUE',
'Maximum model space distance between geometric entities at asserted c
onnectivities');
#18263=UNCERTAINTY_MEASURE_WITH_UNIT(LENGTH_MEASURE(0.01),#18282,
'DISTANCE_ACCURACY_VALUE',
'Maximum model space distance between geometric entities at asserted c
onnectivities');
#18264=UNCERTAINTY_MEASURE_WITH_UNIT(LENGTH_MEASURE(0.01),#18282,
'DISTANCE_ACCURACY_VALUE',
'Maximum model space distance between geometric entities at asserted c
onnectivities');
#18265=UNCERTAINTY_MEASURE_WITH_UNIT(LENGTH_MEASURE(0.01),#18282,
'DISTANCE_ACCURACY_VALUE',
'Maximum model space distance between geometric entities at asserted c
onnectivities');
#18266=UNCERTAINTY_MEASURE_WITH_UNIT(LENGTH_MEASURE(0.01),#18282,
'DISTANCE_ACCURACY_VALUE',
'Maximum model space distance between geometric entities at asserted c
onnectivities');
#18267=(
GEOMETRIC_REPRESENTATION_CONTEXT(3)
GLOBAL_UNCERTAINTY_ASSIGNED_CONTEXT((#18252))
GLOBAL_UNIT_ASSIGNED_CONTEXT((#18282,#18284,#18285))
REPRESENTATION_CONTEXT('','3D')
);
#18268=(
GEOMETRIC_REPRESENTATION_CONTEXT(3)
GLOBAL_UNCERTAINTY_ASSIGNED_CONTEXT((#18253))
GLOBAL_UNIT_ASSIGNED_CONTEXT((#18282,#18284,#18285))
REPRESENTATION_CONTEXT('','3D')
);
#18269=(
GEOMETRIC_REPRESENTATION_CONTEXT(3)
GLOBAL_UNCERTAINTY_ASSIGNED_CONTEXT((#18254))
GLOBAL_UNIT_ASSIGNED_CONTEXT((#18282,#18284,#18285))
REPRESENTATION_CONTEXT('','3D')
);
#18270=(
GEOMETRIC_REPRESENTATION_CONTEXT(3)
GLOBAL_UNCERTAINTY_ASSIGNED_CONTEXT((#18255))
GLOBAL_UNIT_ASSIGNED_CONTEXT((#18282,#18284,#18285))
REPRESENTATION_CONTEXT('','3D')
);
#18271=(
GEOMETRIC_REPRESENTATION_CONTEXT(3)
GLOBAL_UNCERTAINTY_ASSIGNED_CONTEXT((#18256))
GLOBAL_UNIT_ASSIGNED_CONTEXT((#18282,#18284,#18285))
REPRESENTATION_CONTEXT('','3D')
);
#18272=(
GEOMETRIC_REPRESENTATION_CONTEXT(3)
GLOBAL_UNCERTAINTY_ASSIGNED_CONTEXT((#18257))
GLOBAL_UNIT_ASSIGNED_CONTEXT((#18282,#18284,#18285))
REPRESENTATION_CONTEXT('','3D')
);
#18273=(
GEOMETRIC_REPRESENTATION_CONTEXT(3)
GLOBAL_UNCERTAINTY_ASSIGNED_CONTEXT((#18258))
GLOBAL_UNIT_ASSIGNED_CONTEXT((#18282,#18284,#18285))
REPRESENTATION_CONTEXT('','3D')
);
#18274=(
GEOMETRIC_REPRESENTATION_CONTEXT(3)
GLOBAL_UNCERTAINTY_ASSIGNED_CONTEXT((#18259))
GLOBAL_UNIT_ASSIGNED_CONTEXT((#18282,#18284,#18285))
REPRESENTATION_CONTEXT('','3D')
);
#18275=(
GEOMETRIC_REPRESENTATION_CONTEXT(3)
GLOBAL_UNCERTAINTY_ASSIGNED_CONTEXT((#18260))
GLOBAL_UNIT_ASSIGNED_CONTEXT((#18282,#18284,#18285))
REPRESENTATION_CONTEXT('','3D')
);
#18276=(
GEOMETRIC_REPRESENTATION_CONTEXT(3)
GLOBAL_UNCERTAINTY_ASSIGNED_CONTEXT((#18261))
GLOBAL_UNIT_ASSIGNED_CONTEXT((#18282,#18284,#18285))
REPRESENTATION_CONTEXT('','3D')
);
#18277=(
GEOMETRIC_REPRESENTATION_CONTEXT(3)
GLOBAL_UNCERTAINTY_ASSIGNED_CONTEXT((#18262))
GLOBAL_UNIT_ASSIGNED_CONTEXT((#18282,#18284,#18285))
REPRESENTATION_CONTEXT('','3D')
);
#18278=(
GEOMETRIC_REPRESENTATION_CONTEXT(3)
GLOBAL_UNCERTAINTY_ASSIGNED_CONTEXT((#18263))
GLOBAL_UNIT_ASSIGNED_CONTEXT((#18282,#18284,#18285))
REPRESENTATION_CONTEXT('','3D')
);
#18279=(
GEOMETRIC_REPRESENTATION_CONTEXT(3)
GLOBAL_UNCERTAINTY_ASSIGNED_CONTEXT((#18264))
GLOBAL_UNIT_ASSIGNED_CONTEXT((#18282,#18284,#18285))
REPRESENTATION_CONTEXT('','3D')
);
#18280=(
GEOMETRIC_REPRESENTATION_CONTEXT(3)
GLOBAL_UNCERTAINTY_ASSIGNED_CONTEXT((#18265))
GLOBAL_UNIT_ASSIGNED_CONTEXT((#18282,#18284,#18285))
REPRESENTATION_CONTEXT('','3D')
);
#18281=(
GEOMETRIC_REPRESENTATION_CONTEXT(3)
GLOBAL_UNCERTAINTY_ASSIGNED_CONTEXT((#18266))
GLOBAL_UNIT_ASSIGNED_CONTEXT((#18282,#18284,#18285))
REPRESENTATION_CONTEXT('','3D')
);
#18282=(
LENGTH_UNIT()
NAMED_UNIT(*)
SI_UNIT(.MILLI.,.METRE.)
);
#18283=(
LENGTH_UNIT()
NAMED_UNIT(*)
SI_UNIT($,.METRE.)
);
#18284=(
NAMED_UNIT(*)
PLANE_ANGLE_UNIT()
SI_UNIT($,.RADIAN.)
);
#18285=(
NAMED_UNIT(*)
SI_UNIT($,.STERADIAN.)
SOLID_ANGLE_UNIT()
);
#18286=SHAPE_DEFINITION_REPRESENTATION(#18300,#18338);
#18287=SHAPE_DEFINITION_REPRESENTATION(#18301,#18339);
#18288=SHAPE_DEFINITION_REPRESENTATION(#18302,#18340);
#18289=SHAPE_DEFINITION_REPRESENTATION(#18303,#18341);
#18290=SHAPE_DEFINITION_REPRESENTATION(#18304,#18342);
#18291=SHAPE_DEFINITION_REPRESENTATION(#18305,#18343);
#18292=SHAPE_DEFINITION_REPRESENTATION(#18306,#18344);
#18293=SHAPE_DEFINITION_REPRESENTATION(#18307,#18345);
#18294=SHAPE_DEFINITION_REPRESENTATION(#18308,#18346);
#18295=SHAPE_DEFINITION_REPRESENTATION(#18309,#18347);
#18296=SHAPE_DEFINITION_REPRESENTATION(#18310,#18348);
#18297=SHAPE_DEFINITION_REPRESENTATION(#18311,#18349);
#18298=SHAPE_DEFINITION_REPRESENTATION(#18312,#18350);
#18299=SHAPE_DEFINITION_REPRESENTATION(#18313,#18351);
#18300=PRODUCT_DEFINITION_SHAPE('',$,#18353);
#18301=PRODUCT_DEFINITION_SHAPE('',$,#18354);
#18302=PRODUCT_DEFINITION_SHAPE('',$,#18355);
#18303=PRODUCT_DEFINITION_SHAPE('',$,#18356);
#18304=PRODUCT_DEFINITION_SHAPE('',$,#18357);
#18305=PRODUCT_DEFINITION_SHAPE('',$,#18358);
#18306=PRODUCT_DEFINITION_SHAPE('',$,#18359);
#18307=PRODUCT_DEFINITION_SHAPE('',$,#18360);
#18308=PRODUCT_DEFINITION_SHAPE('',$,#18361);
#18309=PRODUCT_DEFINITION_SHAPE('',$,#18362);
#18310=PRODUCT_DEFINITION_SHAPE('',$,#18363);
#18311=PRODUCT_DEFINITION_SHAPE('',$,#18364);
#18312=PRODUCT_DEFINITION_SHAPE('',$,#18365);
#18313=PRODUCT_DEFINITION_SHAPE('',$,#18366);
#18314=PRODUCT_DEFINITION_SHAPE($,$,#83);
#18315=PRODUCT_DEFINITION_SHAPE($,$,#84);
#18316=PRODUCT_DEFINITION_SHAPE($,$,#85);
#18317=PRODUCT_DEFINITION_SHAPE($,$,#86);
#18318=PRODUCT_DEFINITION_SHAPE($,$,#87);
#18319=PRODUCT_DEFINITION_SHAPE($,$,#88);
#18320=PRODUCT_DEFINITION_SHAPE($,$,#89);
#18321=PRODUCT_DEFINITION_SHAPE($,$,#90);
#18322=PRODUCT_DEFINITION_SHAPE($,$,#91);
#18323=PRODUCT_DEFINITION_SHAPE($,$,#92);
#18324=PRODUCT_DEFINITION_SHAPE($,$,#93);
#18325=PRODUCT_DEFINITION_SHAPE($,$,#94);
#18326=PRODUCT_DEFINITION_SHAPE($,$,#95);
#18327=PRODUCT_DEFINITION_SHAPE($,$,#96);
#18328=PRODUCT_DEFINITION_SHAPE($,$,#97);
#18329=PRODUCT_DEFINITION_SHAPE($,$,#98);
#18330=PRODUCT_DEFINITION_SHAPE($,$,#99);
#18331=PRODUCT_DEFINITION_SHAPE($,$,#100);
#18332=PRODUCT_DEFINITION_SHAPE($,$,#101);
#18333=PRODUCT_DEFINITION_SHAPE($,$,#102);
#18334=PRODUCT_DEFINITION_SHAPE($,$,#103);
#18335=PRODUCT_DEFINITION_SHAPE($,$,#104);
#18336=PRODUCT_DEFINITION_SHAPE($,$,#105);
#18337=PRODUCT_DEFINITION_SHAPE($,$,#106);
#18338=SHAPE_REPRESENTATION('',(#9242,#9946,#9947,#9948,#9949,#9950,#9951,
#9952,#9953,#9954,#9955,#9956,#9957,#9958,#9959,#9960,#9961,#9962,#9963,
#9964,#9965,#9966,#9967,#9968,#9969),#18267);
#18339=SHAPE_REPRESENTATION('',(#9243),#18268);
#18340=SHAPE_REPRESENTATION('',(#9277),#18269);
#18341=SHAPE_REPRESENTATION('',(#9302),#18270);
#18342=SHAPE_REPRESENTATION('',(#9470),#18271);
#18343=SHAPE_REPRESENTATION('',(#9544),#18272);
#18344=SHAPE_REPRESENTATION('',(#9664),#18273);
#18345=SHAPE_REPRESENTATION('',(#9674),#18274);
#18346=SHAPE_REPRESENTATION('',(#9696),#18275);
#18347=SHAPE_REPRESENTATION('',(#9713),#18276);
#18348=SHAPE_REPRESENTATION('',(#9729),#18277);
#18349=SHAPE_REPRESENTATION('',(#9847),#18278);
#18350=SHAPE_REPRESENTATION('',(#9884),#18279);
#18351=SHAPE_REPRESENTATION('',(#9936),#18280);
#18352=PRODUCT_DEFINITION_CONTEXT('part definition',#18396,'design');
#18353=PRODUCT_DEFINITION('2026-10-20-13-03-15-172','MAS-286',#18367,#18352);
#18354=PRODUCT_DEFINITION('2026-10-20-13-03-17-896',
'02_Brass_Lower_Centre_Insert',#18368,#18352);
#18355=PRODUCT_DEFINITION('2026-10-20-13-03-18-173',
'13_Brass_Upper_Centre_Insert',#18369,#18352);
#18356=PRODUCT_DEFINITION('2026-10-20-13-03-18-998',
'06_Front_Label_Plate_ON-OFF',#18370,#18352);
#18357=PRODUCT_DEFINITION('2026-10-20-13-03-21-308',
'07_Rear_Cover_Plate',#18371,#18352);
#18358=PRODUCT_DEFINITION('2026-10-20-13-03-16-349',
'01_Pole_Block_Steel',#18372,#18352);
#18359=PRODUCT_DEFINITION('2026-10-20-13-03-18-366',
'03_NdFeB_Rotor_Magnet_D27.8x87.6',#18373,#18352);
#18360=PRODUCT_DEFINITION('2026-10-20-13-03-18-510',
'04_Rotor_Front_Cap_Shaft',#18374,#18352);
#18361=PRODUCT_DEFINITION('2026-10-20-13-03-18-806',
'05_Rotor_Rear_Pivot_Cap',#18375,#18352);
#18362=PRODUCT_DEFINITION('2026-10-20-13-03-22-090',
'08_Flanged_Bushing_10x13x3',#18376,#18352);
#18363=PRODUCT_DEFINITION('2026-10-20-13-03-22-397',
'09_T-Knob_Switch_Handle',#18377,#18352);
#18364=PRODUCT_DEFINITION('2026-10-20-13-03-25-014',
'10_ISO_4026_Set_Screw_M4x4',#18378,#18352);
#18365=PRODUCT_DEFINITION('2026-10-20-13-03-25-859','11_ISO_10642_M3x8',
#18379,#18352);
#18366=PRODUCT_DEFINITION('2026-10-20-13-03-26-880',
'12_ISO_2338_Tie_Pin_5x70',#18380,#18352);
#18367=PRODUCT_DEFINITION_FORMATION('',$,#18398);
#18368=PRODUCT_DEFINITION_FORMATION('',$,#18399);
#18369=PRODUCT_DEFINITION_FORMATION('',$,#18400);
#18370=PRODUCT_DEFINITION_FORMATION('',$,#18401);
#18371=PRODUCT_DEFINITION_FORMATION('',$,#18402);
#18372=PRODUCT_DEFINITION_FORMATION('',$,#18403);
#18373=PRODUCT_DEFINITION_FORMATION('',$,#18404);
#18374=PRODUCT_DEFINITION_FORMATION('',$,#18405);
#18375=PRODUCT_DEFINITION_FORMATION('',$,#18406);
#18376=PRODUCT_DEFINITION_FORMATION('',$,#18407);
#18377=PRODUCT_DEFINITION_FORMATION('',$,#18408);
#18378=PRODUCT_DEFINITION_FORMATION('',$,#18409);
#18379=PRODUCT_DEFINITION_FORMATION('',$,#18410);
#18380=PRODUCT_DEFINITION_FORMATION('',$,#18411);
#18381=PRODUCT_RELATED_PRODUCT_CATEGORY('MAS-286','MAS-286',(#18398));
#18382=PRODUCT_RELATED_PRODUCT_CATEGORY('02_Brass_Lower_Centre_Insert',
'02_Brass_Lower_Centre_Insert',(#18399));
#18383=PRODUCT_RELATED_PRODUCT_CATEGORY('13_Brass_Upper_Centre_Insert',
'13_Brass_Upper_Centre_Insert',(#18400));
#18384=PRODUCT_RELATED_PRODUCT_CATEGORY('06_Front_Label_Plate_ON-OFF',
'06_Front_Label_Plate_ON-OFF',(#18401));
#18385=PRODUCT_RELATED_PRODUCT_CATEGORY('07_Rear_Cover_Plate',
'07_Rear_Cover_Plate',(#18402));
#18386=PRODUCT_RELATED_PRODUCT_CATEGORY('01_Pole_Block_Steel',
'01_Pole_Block_Steel',(#18403));
#18387=PRODUCT_RELATED_PRODUCT_CATEGORY(
'03_NdFeB_Rotor_Magnet_D27.8x87.6','03_NdFeB_Rotor_Magnet_D27.8x87.6',(#18404));
#18388=PRODUCT_RELATED_PRODUCT_CATEGORY('04_Rotor_Front_Cap_Shaft',
'04_Rotor_Front_Cap_Shaft',(#18405));
#18389=PRODUCT_RELATED_PRODUCT_CATEGORY('05_Rotor_Rear_Pivot_Cap',
'05_Rotor_Rear_Pivot_Cap',(#18406));
#18390=PRODUCT_RELATED_PRODUCT_CATEGORY('08_Flanged_Bushing_10x13x3',
'08_Flanged_Bushing_10x13x3',(#18407));
#18391=PRODUCT_RELATED_PRODUCT_CATEGORY('09_T-Knob_Switch_Handle',
'09_T-Knob_Switch_Handle',(#18408));
#18392=PRODUCT_RELATED_PRODUCT_CATEGORY('10_ISO_4026_Set_Screw_M4x4',
'10_ISO_4026_Set_Screw_M4x4',(#18409));
#18393=PRODUCT_RELATED_PRODUCT_CATEGORY('11_ISO_10642_M3x8',
'11_ISO_10642_M3x8',(#18410));
#18394=PRODUCT_RELATED_PRODUCT_CATEGORY('12_ISO_2338_Tie_Pin_5x70',
'12_ISO_2338_Tie_Pin_5x70',(#18411));
#18395=APPLICATION_PROTOCOL_DEFINITION('international standard',
'automotive_design',2009,#18396);
#18396=APPLICATION_CONTEXT(
'Core Data for Automotive Mechanical Design Process');
#18397=PRODUCT_CONTEXT('part definition',#18396,'mechanical');
#18398=PRODUCT('2026-10-20-13-03-15-172','MAS-286',$,(#18397));
#18399=PRODUCT('2026-10-20-13-03-17-896','02_Brass_Lower_Centre_Insert',
$,(#18397));
#18400=PRODUCT('2026-10-20-13-03-18-173','13_Brass_Upper_Centre_Insert',
$,(#18397));
#18401=PRODUCT('2026-10-20-13-03-18-998','06_Front_Label_Plate_ON-OFF',
$,(#18397));
#18402=PRODUCT('2026-10-20-13-03-21-308','07_Rear_Cover_Plate',$,(#18397));
#18403=PRODUCT('2026-10-20-13-03-16-349','01_Pole_Block_Steel',$,(#18397));
#18404=PRODUCT('2026-10-20-13-03-18-366',
'03_NdFeB_Rotor_Magnet_D27.8x87.6',$,(#18397));
#18405=PRODUCT('2026-10-20-13-03-18-510','04_Rotor_Front_Cap_Shaft',$,(#18397));
#18406=PRODUCT('2026-10-20-13-03-18-806','05_Rotor_Rear_Pivot_Cap',$,(#18397));
#18407=PRODUCT('2026-10-20-13-03-22-090','08_Flanged_Bushing_10x13x3',$,
(#18397));
#18408=PRODUCT('2026-10-20-13-03-22-397','09_T-Knob_Switch_Handle',$,(#18397));
#18409=PRODUCT('2026-10-20-13-03-25-014','10_ISO_4026_Set_Screw_M4x4',$,
(#18397));
#18410=PRODUCT('2026-10-20-13-03-25-859','11_ISO_10642_M3x8',$,(#18397));
#18411=PRODUCT('2026-10-20-13-03-26-880','12_ISO_2338_Tie_Pin_5x70',$,(#18397));
#18412=PRESENTATION_STYLE_ASSIGNMENT((#18417));
#18413=PRESENTATION_STYLE_ASSIGNMENT((#18418));
#18414=PRESENTATION_STYLE_ASSIGNMENT((#18419));
#18415=PRESENTATION_STYLE_ASSIGNMENT((#18420));
#18416=PRESENTATION_STYLE_ASSIGNMENT((#18421));
#18417=SURFACE_STYLE_USAGE(.BOTH.,#18422);
#18418=SURFACE_STYLE_USAGE(.BOTH.,#18423);
#18419=SURFACE_STYLE_USAGE(.BOTH.,#18424);
#18420=SURFACE_STYLE_USAGE(.BOTH.,#18425);
#18421=SURFACE_STYLE_USAGE(.BOTH.,#18426);
#18422=SURFACE_SIDE_STYLE('',(#18427));
#18423=SURFACE_SIDE_STYLE('',(#18428));
#18424=SURFACE_SIDE_STYLE('',(#18429));
#18425=SURFACE_SIDE_STYLE('',(#18430));
#18426=SURFACE_SIDE_STYLE('',(#18431));
#18427=SURFACE_STYLE_FILL_AREA(#18432);
#18428=SURFACE_STYLE_FILL_AREA(#18433);
#18429=SURFACE_STYLE_FILL_AREA(#18434);
#18430=SURFACE_STYLE_FILL_AREA(#18435);
#18431=SURFACE_STYLE_FILL_AREA(#18436);
#18432=FILL_AREA_STYLE('Steel - Satin',(#18437));
#18433=FILL_AREA_STYLE('MAS286_ti',(#18438));
#18434=FILL_AREA_STYLE('MAS286_gun',(#18439));
#18435=FILL_AREA_STYLE('MAS286_ss',(#18440));
#18436=FILL_AREA_STYLE('MAS286_al',(#18441));
#18437=FILL_AREA_STYLE_COLOUR('Steel - Satin',#18442);
#18438=FILL_AREA_STYLE_COLOUR('MAS286_ti',#18443);
#18439=FILL_AREA_STYLE_COLOUR('MAS286_gun',#18444);
#18440=FILL_AREA_STYLE_COLOUR('MAS286_ss',#18445);
#18441=FILL_AREA_STYLE_COLOUR('MAS286_al',#18446);
#18442=COLOUR_RGB('Steel - Satin',0.627450980392157,0.627450980392157,0.627450980392157);
#18443=COLOUR_RGB('MAS286_ti',0.549019607843137,0.572549019607843,0.596078431372549);
#18444=COLOUR_RGB('MAS286_gun',0.313725490196078,0.337254901960784,0.364705882352941);
#18445=COLOUR_RGB('MAS286_ss',0.83921568627451,0.850980392156863,0.862745098039216);
#18446=COLOUR_RGB('MAS286_al',0.67843137254902,0.705882352941177,0.729411764705882);
#18447=COLOUR_RGB('Dark Blue',0.08,0.2,0.34);
#18448=FILL_AREA_STYLE_COLOUR('',#18447);
#18449=FILL_AREA_STYLE('',(#18448));
#18450=SURFACE_STYLE_FILL_AREA(#18449);
#18451=SURFACE_SIDE_STYLE('',(#18450));
#18452=SURFACE_STYLE_USAGE(.BOTH.,#18451);
#18453=PRESENTATION_STYLE_ASSIGNMENT((#18452));
#18454=COLOUR_RGB('Light Blue',0.38,0.62,0.78);
#18455=FILL_AREA_STYLE_COLOUR('',#18454);
#18456=FILL_AREA_STYLE('',(#18455));
#18457=SURFACE_STYLE_FILL_AREA(#18456);
#18458=SURFACE_SIDE_STYLE('',(#18457));
#18459=SURFACE_STYLE_USAGE(.BOTH.,#18458);
#18460=PRESENTATION_STYLE_ASSIGNMENT((#18459));
#18461=COLOUR_RGB('Sky Blue',0.24,0.69,0.87);
#18462=FILL_AREA_STYLE_COLOUR('',#18461);
#18463=FILL_AREA_STYLE('',(#18462));
#18464=SURFACE_STYLE_FILL_AREA(#18463);
#18465=SURFACE_SIDE_STYLE('',(#18464));
#18466=SURFACE_STYLE_USAGE(.BOTH.,#18465);
#18467=PRESENTATION_STYLE_ASSIGNMENT((#18466));
#18468=COLOUR_RGB('Grey',0.48,0.52,0.57);
#18469=FILL_AREA_STYLE_COLOUR('',#18468);
#18470=FILL_AREA_STYLE('',(#18469));
#18471=SURFACE_STYLE_FILL_AREA(#18470);
#18472=SURFACE_SIDE_STYLE('',(#18471));
#18473=SURFACE_STYLE_USAGE(.BOTH.,#18472);
#18474=PRESENTATION_STYLE_ASSIGNMENT((#18473));
#18475=COLOUR_RGB('Black',0.12,0.14,0.17);
#18476=FILL_AREA_STYLE_COLOUR('',#18475);
#18477=FILL_AREA_STYLE('',(#18476));
#18478=SURFACE_STYLE_FILL_AREA(#18477);
#18479=SURFACE_SIDE_STYLE('',(#18478));
#18480=SURFACE_STYLE_USAGE(.BOTH.,#18479);
#18481=PRESENTATION_STYLE_ASSIGNMENT((#18480));
#18482=COLOUR_RGB('Off White',0.89,0.88,0.83);
#18483=FILL_AREA_STYLE_COLOUR('',#18482);
#18484=FILL_AREA_STYLE('',(#18483));
#18485=SURFACE_STYLE_FILL_AREA(#18484);
#18486=SURFACE_SIDE_STYLE('',(#18485));
#18487=SURFACE_STYLE_USAGE(.BOTH.,#18486);
#18488=PRESENTATION_STYLE_ASSIGNMENT((#18487));
ENDSEC;
END-ISO-10303-21;
